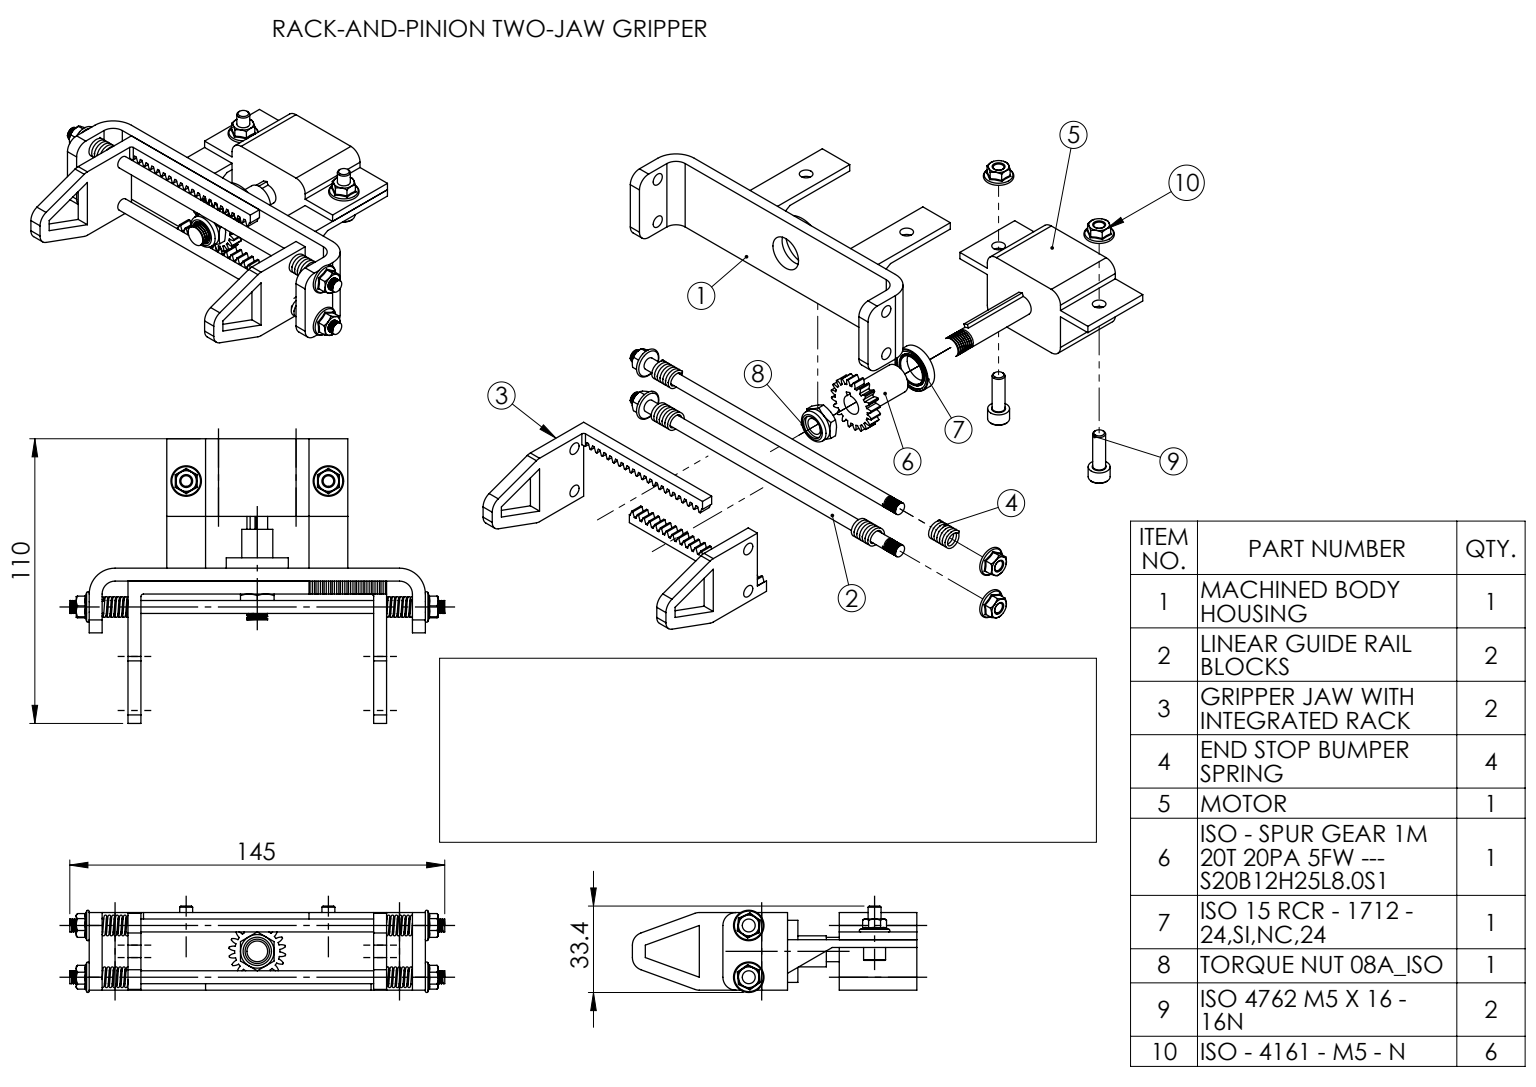
ISO-10303-21;
HEADER;
FILE_DESCRIPTION (('STEP AP214'),
    '1' );
FILE_NAME ('BR-005',
    '2026-10-08T13:46:47',
    ( '' ),
    ( '' ),
    'SwSTEP 2.0',
    'SolidWorks 2026',
    '' );
FILE_SCHEMA (( 'AUTOMOTIVE_DESIGN' ));
ENDSEC;

DATA;
#1 = CARTESIAN_POINT ( 'NONE',  ( -3.999999999999999112, 1.656854249492380804, 17.93750000000000711 ) ) ;
#2 = CARTESIAN_POINT ( 'NONE',  ( -4.000000000000000000, 0.9868501483902560878, -0.09357334158579519445 ) ) ;
#3 = VECTOR ( 'NONE', #11246, 1000.000000000000000 ) ;
#4 = CIRCLE ( 'NONE', #19877, 8.800000000000023803 ) ;
#5 = DIRECTION ( 'NONE',  ( -1.000000000000000000, 0.000000000000000000, -0.000000000000000000 ) ) ;
#6 = DIRECTION ( 'NONE',  ( -0.000000000000000000, -0.000000000000000000, 1.000000000000000000 ) ) ;
#7 = AXIS2_PLACEMENT_3D ( 'NONE', #19593, #12332, #12571 ) ;
#8 = CARTESIAN_POINT ( 'NONE',  ( -67.64999999999999147, 11.03553390593273598, 17.50000000000000355 ) ) ;
#9 = AXIS2_PLACEMENT_3D ( 'NONE', #7701, #5884, #15018 ) ;
#10 = DIRECTION ( 'NONE',  ( -0.000000000000000000, -0.000000000000000000, -1.000000000000000000 ) ) ;
#11 = CARTESIAN_POINT ( 'NONE',  ( 1.432654583217641164, 3.458734125000000326, 19.12500000136560629 ) ) ;
#12 = DIRECTION ( 'NONE',  ( 1.000000000000000000, 0.000000000000000000, 0.000000000000000000 ) ) ;
#13 = CARTESIAN_POINT ( 'NONE',  ( -1.656854249492380804, 4.000000000000000000, 6.112500000000002487 ) ) ;
#14 = ADVANCED_FACE ( 'NONE', ( #23177 ), #19348, .T. ) ;
#15 = DIRECTION ( 'NONE',  ( -1.000000000000000000, 0.000000000000000000, 0.000000000000000000 ) ) ;
#16 = CARTESIAN_POINT ( 'NONE',  ( 2.445694354108821855, -2.445694354108820079, 11.81250000136560629 ) ) ;
#17 = CARTESIAN_POINT ( 'NONE',  ( 65.80000000218494449, 9.999999999999998224, 12.49999999999999289 ) ) ;
#18 = ORIENTED_EDGE ( 'NONE', *, *, #6198, .T. ) ;
#19 = CARTESIAN_POINT ( 'NONE',  ( -69.15000000109247935, 8.538419263543524096, 13.53841926354352054 ) ) ;
#20 = ORIENTED_EDGE ( 'NONE', *, *, #20160, .F. ) ;
#21 = CARTESIAN_POINT ( 'NONE',  ( 57.71643183416158251, 13.97181229448536399, 16.72490539043799629 ) ) ;
#22 = CARTESIAN_POINT ( 'NONE',  ( -68.25000000109247367, 7.933012699999995476, 14.99999999999999645 ) ) ;
#23 = DIRECTION ( 'NONE',  ( 1.000000000000000000, 0.000000000000000000, 0.000000000000000000 ) ) ;
#24 = FACE_OUTER_BOUND ( 'NONE', #11980, .T. ) ;
#25 = VERTEX_POINT ( 'NONE', #5216 ) ;
#26 = VECTOR ( 'NONE', #20577, 1000.000000000000114 ) ;
#27 = EDGE_CURVE ( 'NONE', #6815, #4177, #10288, .T. ) ;
#28 =( GEOMETRIC_REPRESENTATION_CONTEXT ( 3 ) GLOBAL_UNCERTAINTY_ASSIGNED_CONTEXT ( ( #2821 ) ) GLOBAL_UNIT_ASSIGNED_CONTEXT ( ( #14742, #12246, #9459 ) ) REPRESENTATION_CONTEXT ( 'NONE', 'WORKASPACE' ) );
#29 = ORIENTED_EDGE ( 'NONE', *, *, #20734, .T. ) ;
#30 = CARTESIAN_POINT ( 'NONE',  ( -2.449293598294706907E-16, 4.000000000000000000, 7.613708498984758322 ) ) ;
#31 = CARTESIAN_POINT ( 'NONE',  ( 51.40856816583843880, 12.97181229448534978, 13.68930817193506755 ) ) ;
#32 = CARTESIAN_POINT ( 'NONE',  ( -70.40000000109250777, 10.85617417291294551, 17.06698729999999742 ) ) ;
#33 = CARTESIAN_POINT ( 'NONE',  ( -70.80000000109245661, 7.933012699999995476, 15.85617417291294196 ) ) ;
#34 = CARTESIAN_POINT ( 'NONE',  ( -1.432654583217639832, -3.458734125000000326, 12.87500000136560629 ) ) ;
#35 = DIRECTION ( 'NONE',  ( -1.000000000000000000, 0.000000000000000000, 0.000000000000000000 ) ) ;
#36 = CARTESIAN_POINT ( 'NONE',  ( 52.87500000000000711, 7.878679656440349177, 12.87867965644035984 ) ) ;
#37 = CIRCLE ( 'NONE', #17650, 6.543750000000021494 ) ;
#38 = DIRECTION ( 'NONE',  ( -0.000000000000000000, -0.000000000000000000, 1.000000000000000000 ) ) ;
#39 = CARTESIAN_POINT ( 'NONE',  ( 51.09375000000000000, 11.24264068711927322, 11.99999999999998934 ) ) ;
#40 = CARTESIAN_POINT ( 'NONE',  ( -3.999999999999999112, 0.000000000000000000, 16.12500000273119838 ) ) ;
#41 = CARTESIAN_POINT ( 'NONE',  ( -20.00000000000000711, 9.999999999999964473, -19.99999999999999645 ) ) ;
#42 = EDGE_LOOP ( 'NONE', ( #8288, #11668, #9814 ) ) ;
#43 = CARTESIAN_POINT ( 'NONE',  ( 70.34999999999999432, 7.499999999999996447, 13.96446609406725514 ) ) ;
#44 = CYLINDRICAL_SURFACE ( 'NONE', #19665, 4.000000000000000000 ) ;
#45 = ORIENTED_EDGE ( 'NONE', *, *, #7742, .T. ) ;
#46 = CARTESIAN_POINT ( 'NONE',  ( 51.56250000000000711, 6.999999999999997335, 15.00000000000000533 ) ) ;
#47 = CARTESIAN_POINT ( 'NONE',  ( -1.656854249492380804, 4.000000000000000000, -3.762499997268812013 ) ) ;
#48 = EDGE_CURVE ( 'NONE', #4600, #14452, #12227, .T. ) ;
#49 = DIRECTION ( 'NONE',  ( 1.000000000000000000, 0.000000000000000000, 0.000000000000000000 ) ) ;
#50 = ORIENTED_EDGE ( 'NONE', *, *, #19475, .F. ) ;
#51 = CARTESIAN_POINT ( 'NONE',  ( -3.999999999999999112, 1.656854249492380804, 17.93750000000000711 ) ) ;
#52 = CARTESIAN_POINT ( 'NONE',  ( 4.000000000000000000, 4.898587196589412829E-16, -2.199999999999998845 ) ) ;
#53 = CARTESIAN_POINT ( 'NONE',  ( 37.82128094071656932, -8.974600000000002353, 5.000000000000079936 ) ) ;
#54 = ORIENTED_EDGE ( 'NONE', *, *, #9397, .T. ) ;
#55 = LINE ( 'NONE', #5451, #11850 ) ;
#56 = LINE ( 'NONE', #21954, #15596 ) ;
#57 =( BOUNDED_CURVE ( )  B_SPLINE_CURVE ( 2, ( #2610, #2843, #8385, #9828, #929, #6582, #8267, #22849, #6463, #6101, #17122, #17483, #13433, #15701, #13784, #9954, #4303, #22975, #13896, #11639, #18906, #22618, #13542, #6222, #20810, #11753, #17248, #20493, #4334, #741, #505, #18828, #9508, #20729, #17161, #8185, #2415, #386, #851, #13111, #22409, #7826, #15148, #8076, #2169, #17043, #22169, #15387, #5783, #17285, #13469, #19061, #2652, #18588, #20845, #4223, #7945, #20371, #3977, #22286, #6018, #15031, #9746, #619, #18944, #15264, #9995, #7717, #11673, #4452, #2527, #5903, #11314, #13228, #4096, #9867, #13575, #16805, #11436, #18711, #22651, #22534, #2301, #9636, #6257, #16927, #11789, #11559, #13345, #20613, #6145, #10351, #23232, #4923, #21079, #10224, #15739, #2878, #3239, #19639, #8539, #1312, #13695, #13823, #19181, #20955, #6378, #23115, #17398, #12136, #14038, #23010, #4688, #12260, #8652, #1083, #8426, #10464, #2766, #17640, #1430, #6500, #17858, #21428, #22767, #13933, #19527, #15950, #1200 ),
 .UNSPECIFIED., .F., .F. ) 
 B_SPLINE_CURVE_WITH_KNOTS ( ( 3, 2, 2, 2, 2, 2, 2, 2, 2, 2, 2, 2, 2, 2, 2, 2, 2, 2, 2, 2, 2, 2, 2, 2, 2, 2, 2, 2, 2, 2, 2, 2, 2, 2, 2, 2, 2, 2, 2, 2, 2, 2, 2, 2, 2, 2, 2, 2, 2, 2, 2, 2, 2, 2, 2, 2, 2, 2, 2, 2, 2, 2, 2, 2, 3 ),
 ( 0.000000000000000000, 0.01562500000000000000, 0.03125000000000000000, 0.04687500000000000000, 0.06250000000000000000, 0.07812500000000000000, 0.09375000000000000000, 0.1093750000000000000, 0.1250000000000000000, 0.1406250000000000000, 0.1562500000000000000, 0.1718750000000000000, 0.1875000000000000000, 0.2031250000000000000, 0.2187500000000000000, 0.2343750000000000000, 0.2500000000000000000, 0.2656250000000000000, 0.2812500000000000000, 0.2968750000000000000, 0.3125000000000000000, 0.3281250000000000000, 0.3437500000000000000, 0.3593750000000000000, 0.3750000000000000000, 0.3906250000000000000, 0.4062500000000000000, 0.4218750000000000000, 0.4375000000000000000, 0.4531250000000000000, 0.4687500000000000000, 0.4843750000000000000, 0.5000000000000000000, 0.5156250000000000000, 0.5312500000000000000, 0.5468750000000000000, 0.5625000000000000000, 0.5781250000000000000, 0.5937500000000000000, 0.6093750000000000000, 0.6250000000000000000, 0.6406250000000000000, 0.6562500000000000000, 0.6718750000000000000, 0.6875000000000000000, 0.7031250000000000000, 0.7187500000000000000, 0.7343750000000000000, 0.7500000000000000000, 0.7656250000000000000, 0.7812500000000000000, 0.7968750000000000000, 0.8125000000000000000, 0.8281250000000000000, 0.8437500000000000000, 0.8593750000000000000, 0.8750000000000000000, 0.8906250000000000000, 0.9062500000000000000, 0.9218750000000000000, 0.9375000000000000000, 0.9531250000000000000, 0.9687500000000000000, 0.9843750000000000000, 1.000000000000000000 ),
 .UNSPECIFIED. ) 
 CURVE ( )  GEOMETRIC_REPRESENTATION_ITEM ( )  RATIONAL_B_SPLINE_CURVE ( ( 1.000000000000000000, 0.9238795325112867385, 1.000000000000000000, 0.9238795325112867385, 1.000000000000000000, 0.9238795325112867385, 1.000000000000000000, 0.9238795325112867385, 1.000000000000000000, 0.9238795325112867385, 1.000000000000000000, 0.9238795325112867385, 1.000000000000000000, 0.9238795325112867385, 1.000000000000000000, 0.9238795325112867385, 1.000000000000000000, 0.9238795325112867385, 1.000000000000000000, 0.9238795325112867385, 1.000000000000000000, 0.9238795325112867385, 1.000000000000000000, 0.9238795325112867385, 1.000000000000000000, 0.9238795325112867385, 1.000000000000000000, 0.9238795325112867385, 1.000000000000000000, 0.9238795325112867385, 1.000000000000000000, 0.9238795325112867385, 1.000000000000000000, 0.9238795325112867385, 1.000000000000000000, 0.9238795325112867385, 1.000000000000000000, 0.9238795325112867385, 1.000000000000000000, 0.9238795325112867385, 1.000000000000000000, 0.9238795325112867385, 1.000000000000000000, 0.9238795325112867385, 1.000000000000000000, 0.9238795325112867385, 1.000000000000000000, 0.9238795325112867385, 1.000000000000000000, 0.9238795325112867385, 1.000000000000000000, 0.9238795325112867385, 1.000000000000000000, 0.9238795325112867385, 1.000000000000000000, 0.9238795325112867385, 1.000000000000000000, 0.9238795325112867385, 1.000000000000000000, 0.9238795325112867385, 1.000000000000000000, 0.9238795325112867385, 1.000000000000000000, 0.9238795325112867385, 1.000000000000000000, 0.9238795325112867385, 1.000000000000000000, 0.9238795325112867385, 1.000000000000000000, 0.9238795325112867385, 1.000000000000000000, 0.9238795325112867385, 1.000000000000000000, 0.9238795325112867385, 1.000000000000000000, 0.9238795325112867385, 1.000000000000000000, 0.9238795325112867385, 1.000000000000000000, 0.9238795325112867385, 1.000000000000000000, 0.9238795325112867385, 1.000000000000000000, 0.9238795325112867385, 1.000000000000000000, 0.9238795325112867385, 1.000000000000000000, 0.9238795325112867385, 1.000000000000000000, 0.9238795325112867385, 1.000000000000000000, 0.9238795325112867385, 1.000000000000000000, 0.9238795325112867385, 1.000000000000000000, 0.9238795325112867385, 1.000000000000000000, 0.9238795325112867385, 1.000000000000000000, 0.9238795325112867385, 1.000000000000000000, 0.9238795325112867385, 1.000000000000000000, 0.9238795325112867385, 1.000000000000000000, 0.9238795325112867385, 1.000000000000000000, 0.9238795325112867385, 1.000000000000000000, 0.9238795325112867385, 1.000000000000000000, 0.9238795325112867385, 1.000000000000000000, 0.9238795325112867385, 1.000000000000000000, 0.9238795325112867385, 1.000000000000000000, 0.9238795325112867385, 1.000000000000000000, 0.9238795325112867385, 1.000000000000000000, 0.9238795325112867385, 1.000000000000000000, 0.9238795325112867385, 1.000000000000000000, 0.9238795325112867385, 1.000000000000000000, 0.9238795325112867385, 1.000000000000000000 ) ) 
 REPRESENTATION_ITEM ( '' )  );
#58 = CARTESIAN_POINT ( 'NONE',  ( 1.432654583217642053, -3.458734124999999882, 0.3000000013655960140 ) ) ;
#59 = CARTESIAN_POINT ( 'NONE',  ( 68.14999999999999147, 11.03553390593273598, 12.49999999999999289 ) ) ;
#60 = DIRECTION ( 'NONE',  ( -1.000000000000000000, -0.000000000000000000, 0.000000000000000000 ) ) ;
#61 = CARTESIAN_POINT ( 'NONE',  ( -4.000000000000000000, 4.898587196589412829E-16, 19.04999999999996874 ) ) ;
#62 = CARTESIAN_POINT ( 'NONE',  ( 52.25231816583844591, 7.219692298483957771, 17.87654654797633924 ) ) ;
#63 = CARTESIAN_POINT ( 'NONE',  ( 1.432654583217642275, -3.458734124999999437, -1.949999998634404319 ) ) ;
#64 = CARTESIAN_POINT ( 'NONE',  ( -2.445694354108819191, 2.445694354108820523, 10.31250000136560629 ) ) ;
#65 = DIRECTION ( 'NONE',  ( -1.000000000000000000, -0.000000000000000000, -0.000000000000000000 ) ) ;
#66 = CARTESIAN_POINT ( 'NONE',  ( 4.000000000000000000, 4.898587196589412829E-16, -0.1999999999999987899 ) ) ;
#67 = LINE ( 'NONE', #21968, #2877 ) ;
#68 = ORIENTED_EDGE ( 'NONE', *, *, #3329, .T. ) ;
#69 = PLANE ( 'NONE',  #9969 ) ;
#70 = CARTESIAN_POINT ( 'NONE',  ( -15.59503895323380362, -9.000000000000003553, 10.00000000000008882 ) ) ;
#71 = CARTESIAN_POINT ( 'NONE',  ( -72.37500000054622262, 9.999999999999998224, 17.28349365000000049 ) ) ;
#72 = ORIENTED_EDGE ( 'NONE', *, *, #3373, .F. ) ;
#73 = ORIENTED_EDGE ( 'NONE', *, *, #16986, .F. ) ;
#74 = DIRECTION ( 'NONE',  ( 0.000000000000000000, 0.000000000000000000, -1.000000000000000000 ) ) ;
#75 = CARTESIAN_POINT ( 'NONE',  ( 53.43750000000000711, 10.00000000000001776, 18.99999999999999645 ) ) ;
#76 = ORIENTED_EDGE ( 'NONE', *, *, #9529, .F. ) ;
#77 = LINE ( 'NONE', #11129, #17930 ) ;
#78 = ORIENTED_EDGE ( 'NONE', *, *, #18290, .F. ) ;
#79 = CARTESIAN_POINT ( 'NONE',  ( 56.84606816583843880, 8.411196891453267099, 19.02818770551464667 ) ) ;
#80 = AXIS2_PLACEMENT_3D ( 'NONE', #20688, #15213, #18897 ) ;
#81 = CARTESIAN_POINT ( 'NONE',  ( 66.15000000218495302, 11.03553390593273598, 17.50000000000000355 ) ) ;
#82 = ADVANCED_FACE ( 'NONE', ( #16139 ), #13987, .T. ) ;
#83 = DIRECTION ( 'NONE',  ( -1.000000000000000000, 0.000000000000000000, 0.000000000000000000 ) ) ;
#84 = CARTESIAN_POINT ( 'NONE',  ( -16.41397198033274307, -11.25000000000000355, 5.000000000000079936 ) ) ;
#85 = CARTESIAN_POINT ( 'NONE',  ( 2.828427124746190735, -2.828427124746189847, -0.3249999999999971800 ) ) ;
#86 = ORIENTED_EDGE ( 'NONE', *, *, #19557, .T. ) ;
#87 = CARTESIAN_POINT ( 'NONE',  ( -2.828427124746189403, 2.828427124746190291, 10.87500000000001066 ) ) ;
#88 = DIRECTION ( 'NONE',  ( 0.3420201433256622181, 0.9396926207859107594, -6.162975822039141593E-32 ) ) ;
#89 = CARTESIAN_POINT ( 'NONE',  ( 52.27893183416158251, 8.411196891453236901, 10.97181229448535511 ) ) ;
#90 = PLANE ( 'NONE',  #415 ) ;
#91 = EDGE_CURVE ( 'NONE', #13267, #15347, #17804, .T. ) ;
#92 = DIRECTION ( 'NONE',  ( 0.000000000000000000, 0.000000000000000000, -1.000000000000000000 ) ) ;
#93 = CARTESIAN_POINT ( 'NONE',  ( 72.25000000000000000, 12.50000000000000000, 13.96446609406725692 ) ) ;
#94 = LINE ( 'NONE', #22476, #8071 ) ;
#95 = ORIENTED_EDGE ( 'NONE', *, *, #9004, .T. ) ;
#96 = DIRECTION ( 'NONE',  ( -1.000000000000000000, -0.000000000000000000, -0.000000000000000000 ) ) ;
#97 = CARTESIAN_POINT ( 'NONE',  ( 53.25000000000000711, 7.878679656440361612, 17.12132034355964549 ) ) ;
#98 = LINE ( 'NONE', #14992, #12792 ) ;
#99 =( NAMED_UNIT ( * ) PLANE_ANGLE_UNIT ( ) SI_UNIT ( $, .RADIAN. ) );
#100 = ORIENTED_EDGE ( 'NONE', *, *, #5298, .F. ) ;
#101 = DIRECTION ( 'NONE',  ( -0.9396926207859107594, -0.3420201433256623291, 1.540743955509804830E-32 ) ) ;
#102 = LINE ( 'NONE', #22483, #7227 ) ;
#103 = DIRECTION ( 'NONE',  ( 1.224646799147353207E-16, -0.000000000000000000, 1.000000000000000000 ) ) ;
#104 = ORIENTED_EDGE ( 'NONE', *, *, #7323, .T. ) ;
#105 = CARTESIAN_POINT ( 'NONE',  ( 69.74999999999998579, 11.03553390593276262, 12.50000000000001776 ) ) ;
#106 = EDGE_LOOP ( 'NONE', ( #16635, #20382, #2451, #21476 ) ) ;
#107 = CARTESIAN_POINT ( 'NONE',  ( -65.40000000218495302, 9.999999999999998224, 17.49999999999999645 ) ) ;
#108 = CARTESIAN_POINT ( 'NONE',  ( 4.000000000000000888, 4.898587196589412829E-16, 18.50000000000001066 ) ) ;
#109 = CARTESIAN_POINT ( 'NONE',  ( -1.594879469667249916, -11.25000000000000355, 5.000000000000079936 ) ) ;
#110 = EDGE_CURVE ( 'NONE', #1631, #9768, #19532, .T. ) ;
#111 = DIRECTION ( 'NONE',  ( 0.5000000000000006661, 0.8660254037844382635, -0.000000000000000000 ) ) ;
#112 = EDGE_CURVE ( 'NONE', #23518, #15611, #3206, .T. ) ;
#113 = CARTESIAN_POINT ( 'NONE',  ( -3.462118672051860191, 1.261024841198670421, -3.429387741257551081 ) ) ;
#114 =( NAMED_UNIT ( * ) PLANE_ANGLE_UNIT ( ) SI_UNIT ( $, .RADIAN. ) );
#115 = ORIENTED_EDGE ( 'NONE', *, *, #19552, .T. ) ;
#116 = CARTESIAN_POINT ( 'NONE',  ( -66.74999999999998579, 12.50000000000000000, 16.03553390593273420 ) ) ;
#117 = AXIS2_PLACEMENT_3D ( 'NONE', #18833, #4695, #4456 ) ;
#118 = CARTESIAN_POINT ( 'NONE',  ( 66.45000000218495018, 7.499999999999996447, 13.96446609406725514 ) ) ;
#119 = EDGE_CURVE ( 'NONE', #21784, #14801, #1618, .T. ) ;
#120 = CARTESIAN_POINT ( 'NONE',  ( 65.80000000109247082, 7.933012699999995476, 15.85617417291294196 ) ) ;
#121 = CARTESIAN_POINT ( 'NONE',  ( 1.025207404391860050E-15, 3.458734125000000326, 19.18750000136560629 ) ) ;
#122 = DIRECTION ( 'NONE',  ( -1.000000000000000000, -0.000000000000000000, 0.000000000000000000 ) ) ;
#123 = CARTESIAN_POINT ( 'NONE',  ( -4.000000000000000000, 0.000000000000000000, 5.300000000000000711 ) ) ;
#124 = CARTESIAN_POINT ( 'NONE',  ( -3.999999999999999112, 0.000000000000000000, 13.00000000000001066 ) ) ;
#125 = CARTESIAN_POINT ( 'NONE',  ( 1.432654583217641164, 3.458734125000000326, 12.12500000136560629 ) ) ;
#126 = DIRECTION ( 'NONE',  ( 0.000000000000000000, 0.5877852522924743583, -0.8090169943749467851 ) ) ;
#127 = PRODUCT ( 'Linear Guide Rail Blocks', 'Linear Guide Rail Blocks', '', ( #7707 ) ) ;
#128 =( REPRESENTATION_RELATIONSHIP ('NONE','NONE', #8403, #16640 ) REPRESENTATION_RELATIONSHIP_WITH_TRANSFORMATION ( #23106 )SHAPE_REPRESENTATION_RELATIONSHIP( ) );
#129 = VERTEX_POINT ( 'NONE', #3181 ) ;
#130 = CARTESIAN_POINT ( 'NONE',  ( -70.65000000109247935, 7.933012699999995476, 14.99999999999999645 ) ) ;
#131 = ORIENTED_EDGE ( 'NONE', *, *, #16683, .F. ) ;
#132 = CARTESIAN_POINT ( 'NONE',  ( 56.49768183416158962, 12.87654654797631792, 12.21969229848393113 ) ) ;
#133 = CARTESIAN_POINT ( 'NONE',  ( -69.95000000109247651, 8.538419263543522320, 16.46158073645647235 ) ) ;
#134 = DIRECTION ( 'NONE',  ( 0.3420201433256622736, -0.9396926207859106484, -1.232595164407828100E-31 ) ) ;
#135 = ORIENTED_EDGE ( 'NONE', *, *, #23501, .F. ) ;
#136 = CIRCLE ( 'NONE', #7427, 8.749000000000002331 ) ;
#137 = EDGE_CURVE ( 'NONE', #15758, #669, #1279, .T. ) ;
#138 = ORIENTED_EDGE ( 'NONE', *, *, #22563, .F. ) ;
#139 = CARTESIAN_POINT ( 'NONE',  ( 1.025207404391860050E-15, 3.458734125000000770, 19.43750000136560629 ) ) ;
#140 = CARTESIAN_POINT ( 'NONE',  ( 50.84606816583843880, 8.825410453826357582, 18.02818770551464667 ) ) ;
#141 = CARTESIAN_POINT ( 'NONE',  ( -70.30000000109248504, 12.06698730000000275, 15.85617417291294196 ) ) ;
#142 = ADVANCED_FACE ( 'NONE', ( #17693 ), #8211, .T. ) ;
#143 = AXIS2_PLACEMENT_3D ( 'NONE', #14347, #4748, #19821 ) ;
#144 = CARTESIAN_POINT ( 'NONE',  ( -68.90000000109246514, 12.06698730000000275, 15.85617417291294196 ) ) ;
#145 = DIRECTION ( 'NONE',  ( 1.000000000000000000, 0.000000000000000000, 0.000000000000000000 ) ) ;
#146 = CARTESIAN_POINT ( 'NONE',  ( -4.197393957002303999, -0.8151795401431414234, -3.503767560748935139 ) ) ;
#147 = EDGE_CURVE ( 'NONE', #12600, #6989, #10767, .T. ) ;
#148 = CARTESIAN_POINT ( 'NONE',  ( 52.59375000000000711, 11.24264068711927322, 11.99999999999998934 ) ) ;
#149 = DIRECTION ( 'NONE',  ( -0.000000000000000000, 1.000000000000000000, -0.000000000000000000 ) ) ;
#150 = ADVANCED_FACE ( 'NONE', ( #6674 ), #1255, .T. ) ;
#151 = CARTESIAN_POINT ( 'NONE',  ( 53.53125000000000000, 11.24264068711929276, 18.00000000000000355 ) ) ;
#152 = CARTESIAN_POINT ( 'NONE',  ( 2.828427124746191179, 2.828427124746190291, 16.75000000273119838 ) ) ;
#153 = CIRCLE ( 'NONE', #6290, 4.000000000000001776 ) ;
#154 = CARTESIAN_POINT ( 'NONE',  ( 0.000000000000000000, -6.807171995660630692, 6.478011392632865295 ) ) ;
#155 = ORIENTED_EDGE ( 'NONE', *, *, #6433, .T. ) ;
#156 = PLANE ( 'NONE',  #640 ) ;
#157 = DIRECTION ( 'NONE',  ( 0.000000000000000000, -0.5000000000000013323, -0.8660254037844380415 ) ) ;
#158 = VERTEX_POINT ( 'NONE', #14232 ) ;
#159 = CARTESIAN_POINT ( 'NONE',  ( 56.53125000000000711, 11.24264068711929276, 18.00000000000000355 ) ) ;
#160 = SHAPE_REPRESENTATION_RELATIONSHIP ( 'NONE' , 'NONE' ,  #21657, #23316 ) ;
#161 = CARTESIAN_POINT ( 'NONE',  ( -4.000000000000000000, 0.000000000000000000, -3.574999997268813345 ) ) ;
#162 = CARTESIAN_POINT ( 'NONE',  ( 0.000000000000000000, 8.734705317681626724, 0.4999240074894746311 ) ) ;
#163 = EDGE_LOOP ( 'NONE', ( #11926, #9708, #6526, #4328 ) ) ;
#164 = CARTESIAN_POINT ( 'NONE',  ( 1.971781867644420635E-15, -4.000000000000000000, 16.25000000000001066 ) ) ;
#165 = CARTESIAN_POINT ( 'NONE',  ( 0.000000000000000000, 0.4999240074895661690, -8.734705317681621395 ) ) ;
#166 = CARTESIAN_POINT ( 'NONE',  ( 4.999999999999999112, 8.734705317681626724, -0.4999240074894757413 ) ) ;
#167 = ORIENTED_EDGE ( 'NONE', *, *, #18888, .T. ) ;
#168 = DIRECTION ( 'NONE',  ( 0.3420201433256622181, 0.9396926207859107594, -6.162975822039141593E-32 ) ) ;
#169 = DIRECTION ( 'NONE',  ( -1.000000000000000000, 0.000000000000000000, 0.000000000000000000 ) ) ;
#170 = CARTESIAN_POINT ( 'NONE',  ( 67.99999999999998579, 8.232233047033629347, 13.23223304703362402 ) ) ;
#171 = ADVANCED_FACE ( 'NONE', ( #19699 ), #12685, .T. ) ;
#172 = DIRECTION ( 'NONE',  ( 0.000000000000000000, 0.000000000000000000, 1.000000000000000000 ) ) ;
#173 = AXIS2_PLACEMENT_3D ( 'NONE', #18053, #16495, #3661 ) ;
#174 = EDGE_CURVE ( 'NONE', #22879, #11902, #20401, .T. ) ;
#176 = CARTESIAN_POINT ( 'NONE',  ( -1.317756351988340180, 3.857995168970202116, -0.04852650426601388955 ) ) ;
#175 = AXIS2_PLACEMENT_3D ( 'NONE', #8755, #4676, #12125 ) ;
#177 = CARTESIAN_POINT ( 'NONE',  ( 52.43981816583844591, 10.06805114094564857, 19.00000000000000000 ) ) ;
#178 = AXIS2_PLACEMENT_3D ( 'NONE', #2507, #15364, #6234 ) ;
#179 = CARTESIAN_POINT ( 'NONE',  ( -2.445694354108819635, -2.445694354108820523, -1.137499998634402765 ) ) ;
#180 = CARTESIAN_POINT ( 'NONE',  ( 3.458734125000002546, -1.432654583217639610, 15.12500000136560807 ) ) ;
#181 = CARTESIAN_POINT ( 'NONE',  ( 68.60000000218495586, 9.999999999999998224, 17.49999999999999645 ) ) ;
#182 = CARTESIAN_POINT ( 'NONE',  ( 2.500000000000000000, -1.178949249685214307, 2.042000000000001592 ) ) ;
#183 = CARTESIAN_POINT ( 'NONE',  ( 9.920644283265380691E-16, 4.000000000000000000, 16.75000000000001066 ) ) ;
#184 = ORIENTED_EDGE ( 'NONE', *, *, #1140, .T. ) ;
#185 = CARTESIAN_POINT ( 'NONE',  ( 1.656854249492381470, 4.000000000000000000, 11.81250000273119660 ) ) ;
#186 = DIRECTION ( 'NONE',  ( 1.000000000000000000, 7.703719777548943412E-32, 0.000000000000000000 ) ) ;
#187 = DIRECTION ( 'NONE',  ( 0.9396926207859107594, -0.3420201433256623291, 3.697785493223492838E-32 ) ) ;
#188 = EDGE_LOOP ( 'NONE', ( #20058, #4346, #18980, #11606 ) ) ;
#189 = ORIENTED_EDGE ( 'NONE', *, *, #1029, .F. ) ;
#190 = LINE ( 'NONE', #7521, #665 ) ;
#191 =( BOUNDED_CURVE ( )  B_SPLINE_CURVE ( 2, ( #20921, #4538, #19693, #10520, #10408, #17688, #1250, #8589, #23173 ),
 .UNSPECIFIED., .F., .F. ) 
 B_SPLINE_CURVE_WITH_KNOTS ( ( 3, 2, 2, 2, 3 ),
 ( 0.3125000000000002776, 0.3281250000000001665, 0.3437500000000001110, 0.3593750000000000000, 0.3749999999999998890 ),
 .UNSPECIFIED. ) 
 CURVE ( )  GEOMETRIC_REPRESENTATION_ITEM ( )  RATIONAL_B_SPLINE_CURVE ( ( 0.9999999999999986677, 0.9238795325112880708, 1.000000000000000000, 0.9238795325112867385, 1.000000000000000000, 0.9238795325112867385, 1.000000000000000000, 0.9238795325112872936, 0.9999999999999994449 ) ) 
 REPRESENTATION_ITEM ( '' )  );
#192 = CARTESIAN_POINT ( 'NONE',  ( 58.59375000000000711, 11.65685424949236015, 10.99999999999998579 ) ) ;
#193 = ORIENTED_EDGE ( 'NONE', *, *, #20761, .T. ) ;
#194 = CARTESIAN_POINT ( 'NONE',  ( -2.828427124746188515, -2.828427124746190735, 18.12500000000001066 ) ) ;
#195 = ORIENTED_EDGE ( 'NONE', *, *, #4034, .T. ) ;
#196 = CARTESIAN_POINT ( 'NONE',  ( 54.97106816583843880, 5.971812294485345340, 13.41119689145326710 ) ) ;
#197 = AXIS2_PLACEMENT_3D ( 'NONE', #16444, #18702, #9272 ) ;
#198 = CARTESIAN_POINT ( 'NONE',  ( 70.50000000109247367, 9.143825827087049163, 17.06698729999999742 ) ) ;
#199 = CARTESIAN_POINT ( 'NONE',  ( -2.000000000000001776, 8.130889342088984924E-16, 6.543750000000021494 ) ) ;
#200 = CARTESIAN_POINT ( 'NONE',  ( 70.75000000109247367, 8.538419263543522320, 16.46158073645647235 ) ) ;
#201 = ORIENTED_EDGE ( 'NONE', *, *, #13509, .T. ) ;
#202 = CARTESIAN_POINT ( 'NONE',  ( 9.920644283265380691E-16, 4.000000000000000000, 15.87500000273119660 ) ) ;
#203 = CARTESIAN_POINT ( 'NONE',  ( -2.449293598294706907E-16, 4.000000000000000000, 0.1750000027311865991 ) ) ;
#204 = CARTESIAN_POINT ( 'NONE',  ( 56.49768183416158962, 12.87654654797631792, 12.21969229848393113 ) ) ;
#205 = CARTESIAN_POINT ( 'NONE',  ( 33.85151041966726382, -11.25000000000000355, 5.000000000000079936 ) ) ;
#206 = DIRECTION ( 'NONE',  ( -1.000000000000000000, -0.000000000000000000, -0.000000000000000000 ) ) ;
#207 = CARTESIAN_POINT ( 'NONE',  ( -2.762848947613220307, 4.746226468750993632, -19.99999999999999645 ) ) ;
#208 = CARTESIAN_POINT ( 'NONE',  ( 4.000000000000000000, -2.471525695159793035, -3.686886880705770864 ) ) ;
#209 = ORIENTED_EDGE ( 'NONE', *, *, #10563, .F. ) ;
#210 = LINE ( 'NONE', #7541, #1252 ) ;
#211 = CARTESIAN_POINT ( 'NONE',  ( -4.000000000000000000, -0.8232339106130515116, -3.430630286862743183 ) ) ;
#212 = AXIS2_PLACEMENT_3D ( 'NONE', #2091, #18271, #1855 ) ;
#213 = DIRECTION ( 'NONE',  ( -1.000000000000000000, -0.000000000000000000, 0.000000000000000000 ) ) ;
#214 = PRESENTATION_STYLE_ASSIGNMENT (( #11263 ) ) ;
#215 = ORIENTED_EDGE ( 'NONE', *, *, #13747, .F. ) ;
#216 = EDGE_CURVE ( 'NONE', #1719, #20740, #5490, .T. ) ;
#217 = DIRECTION ( 'NONE',  ( 1.000000000000000000, 0.000000000000000000, 0.000000000000000000 ) ) ;
#218 = CARTESIAN_POINT ( 'NONE',  ( 70.54999999999999716, 11.03553390593272177, 12.49999999999998046 ) ) ;
#219 = CARTESIAN_POINT ( 'NONE',  ( 5.000000000000002665, 3.306546357697854226E-16, 2.700000000000000622 ) ) ;
#220 = DIRECTION ( 'NONE',  ( 1.000000000000000000, -0.000000000000000000, -0.000000000000000000 ) ) ;
#221 = ORIENTED_EDGE ( 'NONE', *, *, #20920, .F. ) ;
#222 = CARTESIAN_POINT ( 'NONE',  ( 4.000000000000000000, 2.309401076758497151, -3.433295621305379353 ) ) ;
#223 = ORIENTED_EDGE ( 'NONE', *, *, #14244, .T. ) ;
#224 = CARTESIAN_POINT ( 'NONE',  ( -19.99999999999999645, -9.000000000000003553, 5.000000000000079936 ) ) ;
#225 = CARTESIAN_POINT ( 'NONE',  ( 4.000000000000000888, 4.898587196589412829E-16, 15.50000000000001066 ) ) ;
#226 = DIRECTION ( 'NONE',  ( -1.000000000000000000, -0.000000000000000000, 0.000000000000000000 ) ) ;
#227 = FACE_OUTER_BOUND ( 'NONE', #6243, .T. ) ;
#228 = DIRECTION ( 'NONE',  ( 0.000000000000000000, 0.000000000000000000, -1.000000000000000000 ) ) ;
#229 = CARTESIAN_POINT ( 'NONE',  ( 71.25000000109247367, 12.06698730000000097, 14.99999999999999645 ) ) ;
#230 = ORIENTED_EDGE ( 'NONE', *, *, #2307, .F. ) ;
#231 = CARTESIAN_POINT ( 'NONE',  ( -68.54999999999999716, 8.964466094067258695, 17.50000000000000355 ) ) ;
#232 = DIRECTION ( 'NONE',  ( -0.000000000000000000, -0.000000000000000000, 1.000000000000000000 ) ) ;
#233 = CARTESIAN_POINT ( 'NONE',  ( 66.95000000109246230, 11.46158073645647235, 13.53841926354352232 ) ) ;
#234 = CARTESIAN_POINT ( 'NONE',  ( 1.432654583217643163, -3.458734124999999437, 15.75000000136560629 ) ) ;
#235 = CARTESIAN_POINT ( 'NONE',  ( -4.898587196589412829E-16, 0.000000000000000000, -4.000000000000000000 ) ) ;
#236 = CARTESIAN_POINT ( 'NONE',  ( 1.432654583217642275, -3.458734124999999882, -2.699999998634404541 ) ) ;
#237 = CARTESIAN_POINT ( 'NONE',  ( -2.828427124746190291, 2.828427124746190291, 6.175000000000001599 ) ) ;
#238 = CARTESIAN_POINT ( 'NONE',  ( -3.458734124999998993, 1.432654583217640276, 12.37500000136560629 ) ) ;
#239 = DIRECTION ( 'NONE',  ( -1.000000000000000000, 0.000000000000000000, 0.000000000000000000 ) ) ;
#240 = ORIENTED_EDGE ( 'NONE', *, *, #11094, .F. ) ;
#241 = EDGE_CURVE ( 'NONE', #1931, #14063, #136, .T. ) ;
#242 = CARTESIAN_POINT ( 'NONE',  ( -69.65000000109247935, 9.999999999999998224, 17.06698730000000097 ) ) ;
#243 = ORIENTED_EDGE ( 'NONE', *, *, #7766, .T. ) ;
#244 = CARTESIAN_POINT ( 'NONE',  ( 55.93518183416157541, 9.931948859054379852, 18.99999999999999289 ) ) ;
#245 = CARTESIAN_POINT ( 'NONE',  ( -71.80000000109245661, 9.143825827087050939, 12.93301269999999370 ) ) ;
#246 = APPLICATION_PROTOCOL_DEFINITION ( 'draft international standard', 'automotive_design', 1998, #4859 ) ;
#247 = EDGE_CURVE ( 'NONE', #438, #3610, #9877, .T. ) ;
#248 = LINE ( 'NONE', #7582, #20083 ) ;
#249 = ORIENTED_EDGE ( 'NONE', *, *, #5499, .T. ) ;
#250 = ORIENTED_EDGE ( 'NONE', *, *, #1042, .T. ) ;
#251 = CARTESIAN_POINT ( 'NONE',  ( 3.458734125000001658, 1.432654583217640498, 17.25000000136560629 ) ) ;
#252 = EDGE_CURVE ( 'NONE', #16322, #3084, #16594, .T. ) ;
#253 = CARTESIAN_POINT ( 'NONE',  ( 54.56250000000000711, 6.999999999999997335, 15.00000000000000533 ) ) ;
#254 = CARTESIAN_POINT ( 'NONE',  ( -70.50000000109247367, 9.143825827087049163, 17.06698729999999742 ) ) ;
#255 = CIRCLE ( 'NONE', #4097, 8.749000000000002331 ) ;
#256 = CARTESIAN_POINT ( 'NONE',  ( -69.15000000109246514, 8.538419263543522320, 16.46158073645647235 ) ) ;
#257 = CARTESIAN_POINT ( 'NONE',  ( 3.458734125000001658, 1.432654583217640498, 13.25000000136560274 ) ) ;
#258 = PLANE ( 'NONE',  #11121 ) ;
#259 = CARTESIAN_POINT ( 'NONE',  ( 59.96643183416158251, 7.028187705514638672, 13.68930817193508531 ) ) ;
#260 = CARTESIAN_POINT ( 'NONE',  ( -71.70000000000000284, 9.999999999999998224, 17.49999999999999645 ) ) ;
#261 =( REPRESENTATION_RELATIONSHIP ('NONE','NONE', #8403, #20612 ) REPRESENTATION_RELATIONSHIP_WITH_TRANSFORMATION ( #13103 )SHAPE_REPRESENTATION_RELATIONSHIP( ) );
#262 = CARTESIAN_POINT ( 'NONE',  ( 54.28125000000000000, 8.757359312880703683, 11.99999999999999822 ) ) ;
#263 = CARTESIAN_POINT ( 'NONE',  ( -1.432654583217638944, 3.458734125000000326, 12.25000000136560629 ) ) ;
#264 = CARTESIAN_POINT ( 'NONE',  ( 4.000000000000001776, -1.656854249492379694, 16.56250000273119838 ) ) ;
#265 = DIRECTION ( 'NONE',  ( -1.000000000000000000, 0.000000000000000000, 0.000000000000000000 ) ) ;
#266 = AXIS2_PLACEMENT_3D ( 'NONE', #5948, #13273, #13627 ) ;
#267 = AXIS2_PLACEMENT_3D ( 'NONE', #23534, #5337, #9303 ) ;
#268 = EDGE_LOOP ( 'NONE', ( #17451, #14337, #19038, #18297, #4703 ) ) ;
#269 = CARTESIAN_POINT ( 'NONE',  ( 5.200000000000002842, 0.000000000000000000, 0.000000000000000000 ) ) ;
#270 = EDGE_CURVE ( 'NONE', #13563, #6956, #18497, .T. ) ;
#271 = CYLINDRICAL_SURFACE ( 'NONE', #5922, 4.714285714285714413 ) ;
#272 = ORIENTED_EDGE ( 'NONE', *, *, #1937, .F. ) ;
#273 = CARTESIAN_POINT ( 'NONE',  ( 56.15625000000002132, 7.000000000000003553, 16.24264068711929099 ) ) ;
#274 = CARTESIAN_POINT ( 'NONE',  ( 3.458734125000000770, -1.432654583217639610, 4.175000001365593683 ) ) ;
#275 = ADVANCED_FACE ( 'NONE', ( #14703 ), #22200, .F. ) ;
#276 = FACE_OUTER_BOUND ( 'NONE', #8026, .T. ) ;
#277 = EDGE_LOOP ( 'NONE', ( #17839, #20951 ) ) ;
#278 = CARTESIAN_POINT ( 'NONE',  ( 4.000000000000001776, -1.656854249492379694, 13.43750000000001243 ) ) ;
#279 = LINE ( 'NONE', #14812, #13339 ) ;
#280 = LINE ( 'NONE', #14938, #18655 ) ;
#281 = ORIENTED_EDGE ( 'NONE', *, *, #12290, .F. ) ;
#282 = ADVANCED_FACE ( 'NONE', ( #9074 ), #16365, .T. ) ;
#283 = ADVANCED_FACE ( 'NONE', ( #1848 ), #11347, .T. ) ;
#284 = VECTOR ( 'NONE', #13283, 1000.000000000000000 ) ;
#285 = DIRECTION ( 'NONE',  ( -0.000000000000000000, -0.000000000000000000, -1.000000000000000000 ) ) ;
#286 = DIRECTION ( 'NONE',  ( 0.000000000000000000, 0.000000000000000000, -1.000000000000000000 ) ) ;
#287 = AXIS2_PLACEMENT_3D ( 'NONE', #3170, #5332, #9063 ) ;
#288 = AXIS2_PLACEMENT_3D ( 'NONE', #14869, #22247, #466 ) ;
#289 = CARTESIAN_POINT ( 'NONE',  ( 69.14999999999999147, 12.50000000000000000, 16.03553390593273420 ) ) ;
#290 = FACE_OUTER_BOUND ( 'NONE', #18662, .T. ) ;
#291 = DIRECTION ( 'NONE',  ( -1.000000000000000000, 0.000000000000000000, 0.000000000000000000 ) ) ;
#292 = CARTESIAN_POINT ( 'NONE',  ( 59.00231816583843170, 12.07320092032949610, 12.83056023321021044 ) ) ;
#293 = CARTESIAN_POINT ( 'NONE',  ( 3.458734125000000326, 1.432654583217640498, 0.3000000013655960696 ) ) ;
#294 = CARTESIAN_POINT ( 'NONE',  ( 1.432654583217641386, 3.458734125000000770, 13.37500000136560452 ) ) ;
#295 = CARTESIAN_POINT ( 'NONE',  ( 0.000000000000000000, -10.82112760146737962, 1.975651141462196225 ) ) ;
#296 = DIRECTION ( 'NONE',  ( -0.000000000000000000, -1.000000000000000000, -0.000000000000000000 ) ) ;
#297 = VECTOR ( 'NONE', #11394, 1000.000000000000000 ) ;
#298 = CARTESIAN_POINT ( 'NONE',  ( -2.500000000000000444, 3.061616997868383634E-16, -5.000000000000000888 ) ) ;
#299 = VERTEX_POINT ( 'NONE', #11106 ) ;
#300 = DIRECTION ( 'NONE',  ( 0.000000000000000000, 0.000000000000000000, -1.000000000000000000 ) ) ;
#301 = DIRECTION ( 'NONE',  ( -1.000000000000000000, -0.000000000000000000, -0.000000000000000000 ) ) ;
#302 = EDGE_CURVE ( 'NONE', #23443, #22486, #15470, .T. ) ;
#303 = CARTESIAN_POINT ( 'NONE',  ( -2.247776618166699603, 3.308700692843501656, 21.31370849898476649 ) ) ;
#304 = ORIENTED_EDGE ( 'NONE', *, *, #3176, .T. ) ;
#305 = B_SPLINE_CURVE_WITH_KNOTS ( 'NONE', 3,
 ( #22141, #7915, #17258, #22261, #2503 ),
 .UNSPECIFIED., .F., .F.,
 ( 4, 1, 4 ),
 ( 0.000000000000000000, 0.002309401076758506657, 0.004618802153517013315 ),
 .UNSPECIFIED. ) ;
#306 = AXIS2_PLACEMENT_3D ( 'NONE', #17570, #1367, #5089 ) ;
#307 = ORIENTED_EDGE ( 'NONE', *, *, #9563, .T. ) ;
#308 = AXIS2_PLACEMENT_3D ( 'NONE', #22558, #8314, #14060 ) ;
#309 = FILL_AREA_STYLE ('',( #2348 ) ) ;
#310 = EDGE_CURVE ( 'NONE', #17992, #7710, #5573, .T. ) ;
#311 = PRESENTATION_LAYER_ASSIGNMENT (  '', '', ( #14103 ) ) ;
#312 = CARTESIAN_POINT ( 'NONE',  ( 54.37500000000000711, 7.171572875253794166, 12.17157287525381726 ) ) ;
#313 = VERTEX_POINT ( 'NONE', #3887 ) ;
#314 = CARTESIAN_POINT ( 'NONE',  ( -6.500000000000000000, -3.752776749732573247, -0.5805565836007695601 ) ) ;
#315 = VERTEX_POINT ( 'NONE', #10985 ) ;
#316 = EDGE_CURVE ( 'NONE', #22906, #15640, #20161, .T. ) ;
#317 = CARTESIAN_POINT ( 'NONE',  ( 51.78356816583844591, 8.275094609561968184, 11.02818770551464667 ) ) ;
#318 = CARTESIAN_POINT ( 'NONE',  ( 70.70000000109247651, 7.933012699999995476, 14.14382582708705094 ) ) ;
#319 = CARTESIAN_POINT ( 'NONE',  ( 66.49999999999998579, 9.999999999999998224, 12.49999999999999289 ) ) ;
#320 = CARTESIAN_POINT ( 'NONE',  ( 71.55000000109245661, 8.538419263543522320, 16.46158073645647235 ) ) ;
#321 = PRODUCT_DEFINITION_SHAPE ( 'NONE', 'NONE',  #23701 ) ;
#322 = ORIENTED_EDGE ( 'NONE', *, *, #7035, .T. ) ;
#323 = CARTESIAN_POINT ( 'NONE',  ( 1.656854249492384135, -3.999999999999999112, 17.43750000273119483 ) ) ;
#324 = CARTESIAN_POINT ( 'NONE',  ( -2.828427124746190291, 2.828427124746190291, 0.3000000027311867101 ) ) ;
#325 = VECTOR ( 'NONE', #2577, 1000.000000000000000 ) ;
#326 = CARTESIAN_POINT ( 'NONE',  ( 53.21643183416158251, 13.97181229448536399, 16.72490539043799629 ) ) ;
#327 = CARTESIAN_POINT ( 'NONE',  ( 40.13469571966727045, -11.25000000000000355, 10.00000000000008882 ) ) ;
#328 = CARTESIAN_POINT ( 'NONE',  ( 2.499999999999999556, 1.464956435139542323, 10.90201369670499076 ) ) ;
#329 = CARTESIAN_POINT ( 'NONE',  ( 27.50000000000000000, 1.500000000000003109, -33.66025403784446723 ) ) ;
#330 = CARTESIAN_POINT ( 'NONE',  ( 1.656854249492383024, -3.999999999999999112, 0.6125000000000022649 ) ) ;
#331 = CARTESIAN_POINT ( 'NONE',  ( -1.301042606982605321E-15, 7.505553499465137612, -0.5805565836007695601 ) ) ;
#332 = ORIENTED_EDGE ( 'NONE', *, *, #12450, .T. ) ;
#333 = CARTESIAN_POINT ( 'NONE',  ( -70.20000000218495018, 9.999999999999998224, 17.49999999999999645 ) ) ;
#334 = CARTESIAN_POINT ( 'NONE',  ( -4.211399284164270895, 2.459729995988205964, -3.751162237960538715 ) ) ;
#335 = FACE_OUTER_BOUND ( 'NONE', #5328, .T. ) ;
#336 = AXIS2_PLACEMENT_3D ( 'NONE', #17862, #16313, #17643 ) ;
#337 = ORIENTED_EDGE ( 'NONE', *, *, #22086, .T. ) ;
#338 = VECTOR ( 'NONE', #6203, 1000.000000000000000 ) ;
#339 = CARTESIAN_POINT ( 'NONE',  ( 4.999999999999999112, 0.000000000000000000, 0.000000000000000000 ) ) ;
#340 = CARTESIAN_POINT ( 'NONE',  ( -19.99999999999999645, -9.000000000000003553, 5.000000000000079936 ) ) ;
#341 = DIRECTION ( 'NONE',  ( 1.000000000000000000, 0.000000000000000000, 0.000000000000000000 ) ) ;
#342 = EDGE_CURVE ( 'NONE', #20113, #6042, #11222, .T. ) ;
#343 = CARTESIAN_POINT ( 'NONE',  ( 1.656854249492384135, -3.999999999999999112, 16.43750000273119838 ) ) ;
#344 = ORIENTED_EDGE ( 'NONE', *, *, #2171, .T. ) ;
#345 = CARTESIAN_POINT ( 'NONE',  ( -4.471005642132689140, -3.347908285648603766, 10.00000000000008882 ) ) ;
#346 = ORIENTED_EDGE ( 'NONE', *, *, #8932, .T. ) ;
#347 =( GEOMETRIC_REPRESENTATION_CONTEXT ( 3 ) GLOBAL_UNCERTAINTY_ASSIGNED_CONTEXT ( ( #4745 ) ) GLOBAL_UNIT_ASSIGNED_CONTEXT ( ( #17997, #14301, #12516 ) ) REPRESENTATION_CONTEXT ( 'NONE', 'WORKASPACE' ) );
#348 = DIRECTION ( 'NONE',  ( 0.000000000000000000, 1.000000000000000000, -0.000000000000000000 ) ) ;
#349 = VECTOR ( 'NONE', #3642, 1000.000000000000000 ) ;
#350 = CARTESIAN_POINT ( 'NONE',  ( -2.828427124746189403, 2.828427124746190291, 12.87500000000001066 ) ) ;
#351 = DIRECTION ( 'NONE',  ( 0.000000000000000000, 0.000000000000000000, 1.000000000000000000 ) ) ;
#352 = CARTESIAN_POINT ( 'NONE',  ( 2.149474931388133836, 6.264553569211843254, -3.644669744206378681 ) ) ;
#353 = PLANE ( 'NONE',  #2572 ) ;
#354 = CARTESIAN_POINT ( 'NONE',  ( 69.75000000109245946, 11.46158073645647235, 16.46158073645647235 ) ) ;
#355 = AXIS2_PLACEMENT_3D ( 'NONE', #12842, #20101, #14526 ) ;
#356 = ORIENTED_EDGE ( 'NONE', *, *, #112, .T. ) ;
#357 = VECTOR ( 'NONE', #88, 1000.000000000000114 ) ;
#358 = CARTESIAN_POINT ( 'NONE',  ( -90.00000000000000000, 0.000000000000000000, 0.000000000000000000 ) ) ;
#359 = CARTESIAN_POINT ( 'NONE',  ( 0.000000000000000000, 0.000000000000000000, 0.000000000000000000 ) ) ;
#360 = CARTESIAN_POINT ( 'NONE',  ( 65.75000000109247367, 8.538419263543522320, 16.46158073645647235 ) ) ;
#361 = CARTESIAN_POINT ( 'NONE',  ( 1.025207404391860050E-15, 3.458734125000000326, 17.18750000136560274 ) ) ;
#362 = DIRECTION ( 'NONE',  ( -0.000000000000000000, -1.000000000000000000, -0.000000000000000000 ) ) ;
#363 = CARTESIAN_POINT ( 'NONE',  ( -2.445694354108820523, 2.445694354108820523, -2.137499998634403653 ) ) ;
#364 = AXIS2_PLACEMENT_3D ( 'NONE', #4231, #22417, #9754 ) ;
#365 = CARTESIAN_POINT ( 'NONE',  ( 4.000000000000000000, 1.656854249492381248, 1.862500000000001599 ) ) ;
#366 = CARTESIAN_POINT ( 'NONE',  ( -71.30000000218494449, 8.232233047033629347, 13.23223304703362402 ) ) ;
#367 = CARTESIAN_POINT ( 'NONE',  ( -2.445694354108819191, 2.445694354108820523, 15.31250000136560452 ) ) ;
#368 = CYLINDRICAL_SURFACE ( 'NONE', #9, 8.749000000000002331 ) ;
#369 = EDGE_LOOP ( 'NONE', ( #10172, #18701, #9343, #9622 ) ) ;
#370 = CARTESIAN_POINT ( 'NONE',  ( -68.10000000109248219, 9.143825827087049163, 17.06698730000000097 ) ) ;
#371 = ORIENTED_EDGE ( 'NONE', *, *, #16704, .T. ) ;
#372 = CARTESIAN_POINT ( 'NONE',  ( 57.18750000000000000, 9.999999999999978684, 10.99999999999999645 ) ) ;
#373 = CARTESIAN_POINT ( 'NONE',  ( -71.90000000109246514, 10.85617417291294551, 12.93301269999999370 ) ) ;
#374 = SHAPE_DEFINITION_REPRESENTATION ( #9332, #13579 ) ;
#375 = VERTEX_POINT ( 'NONE', #16712 ) ;
#376 = CARTESIAN_POINT ( 'NONE',  ( -2.828427124746190291, 2.828427124746190291, 1.300000002731187543 ) ) ;
#377 = ORIENTED_EDGE ( 'NONE', *, *, #743, .F. ) ;
#378 = VECTOR ( 'NONE', #16810, 1000.000000000000114 ) ;
#379 = VECTOR ( 'NONE', #18858, 1000.000000000000000 ) ;
#380 = ORIENTED_EDGE ( 'NONE', *, *, #8945, .F. ) ;
#381 = CARTESIAN_POINT ( 'NONE',  ( 1.432654583217641386, 3.458734125000000770, 15.37500000136560807 ) ) ;
#382 = CARTESIAN_POINT ( 'NONE',  ( 53.43750000000000711, 10.00000000000000711, 17.99999999999999645 ) ) ;
#383 = VECTOR ( 'NONE', #917, 1000.000000000000000 ) ;
#384 = CARTESIAN_POINT ( 'NONE',  ( -67.50000000109247367, 7.933012699999995476, 14.14382582708705094 ) ) ;
#385 = AXIS2_PLACEMENT_3D ( 'NONE', #6028, #512, #265 ) ;
#386 = CARTESIAN_POINT ( 'NONE',  ( 70.20000000109246230, 12.06698729999999919, 14.14382582708705094 ) ) ;
#387 = ADVANCED_FACE ( 'NONE', ( #290 ), #419, .F. ) ;
#388 = CARTESIAN_POINT ( 'NONE',  ( -67.75000000109245946, 8.538419263543524096, 13.53841926354352054 ) ) ;
#389 = CARTESIAN_POINT ( 'NONE',  ( 2.445694354108822299, -2.445694354108820079, 12.06250000136560629 ) ) ;
#390 = CARTESIAN_POINT ( 'NONE',  ( 18.14354716966726144, -11.25000000000000355, 10.00000000000008882 ) ) ;
#391 = CARTESIAN_POINT ( 'NONE',  ( 55.65393183416158251, 6.971812294485357775, 16.17458954617365663 ) ) ;
#392 = CARTESIAN_POINT ( 'NONE',  ( -9.000000000000000000, 1.102182119232617714E-15, 1.102182119232617714E-15 ) ) ;
#393 = CARTESIAN_POINT ( 'NONE',  ( 55.21875000000000000, 13.00000000000000711, 16.24264068711927322 ) ) ;
#394 = CARTESIAN_POINT ( 'NONE',  ( 6.625378842019205905, 0.6908453745559488546, 10.00000000000008882 ) ) ;
#395 = CARTESIAN_POINT ( 'NONE',  ( -3.999999999999999112, 0.000000000000000000, 17.12500000273119838 ) ) ;
#396 = EDGE_CURVE ( 'NONE', #2255, #17303, #7746, .T. ) ;
#397 = DIRECTION ( 'NONE',  ( -1.848892746611742040E-32, -0.3420201433256690460, 0.9396926207859083169 ) ) ;
#398 = AXIS2_PLACEMENT_3D ( 'NONE', #11529, #8386, #10076 ) ;
#399 = ORIENTED_EDGE ( 'NONE', *, *, #10605, .F. ) ;
#400 = CARTESIAN_POINT ( 'NONE',  ( 70.39999999999999147, 8.232233047033629347, 13.23223304703362402 ) ) ;
#401 = CARTESIAN_POINT ( 'NONE',  ( 1.519999999999999574, 0.000000000000000000, -6.760799999999997034 ) ) ;
#402 = VERTEX_POINT ( 'NONE', #20872 ) ;
#403 = CARTESIAN_POINT ( 'NONE',  ( 56.31018183416157541, 12.99999999999999822, 15.06805114094562192 ) ) ;
#405 = COLOUR_RGB ( '', 0.66274510, 0.83137255, 0.94901961) ;
#404 = APPLICATION_PROTOCOL_DEFINITION ( 'draft international standard', 'automotive_design', 1998, #10237 ) ;
#406 = CARTESIAN_POINT ( 'NONE',  ( 4.000000000000000000, 1.656854249492381248, -2.012499997268811569 ) ) ;
#407 = DIRECTION ( 'NONE',  ( 0.000000000000000000, 0.000000000000000000, -1.000000000000000000 ) ) ;
#408 = ORIENTED_EDGE ( 'NONE', *, *, #13246, .T. ) ;
#409 = CARTESIAN_POINT ( 'NONE',  ( 4.000000000000001776, -1.656854249492379694, 12.43750000000001066 ) ) ;
#410 = DIRECTION ( 'NONE',  ( -1.000000000000000000, 0.000000000000000000, -0.000000000000000000 ) ) ;
#411 = DIRECTION ( 'NONE',  ( 0.000000000000000000, 0.000000000000000000, -1.000000000000000000 ) ) ;
#412 = ORIENTED_EDGE ( 'NONE', *, *, #302, .T. ) ;
#413 = CARTESIAN_POINT ( 'NONE',  ( -70.80000000218494449, 12.50000000000000000, 14.99999999999999645 ) ) ;
#414 = CARTESIAN_POINT ( 'NONE',  ( -3.458734125000000326, -1.432654583217642497, 1.050000001365596791 ) ) ;
#415 = AXIS2_PLACEMENT_3D ( 'NONE', #22234, #2115, #9450 ) ;
#416 = ADVANCED_FACE ( 'NONE', ( #532 ), #16955, .F. ) ;
#417 = CARTESIAN_POINT ( 'NONE',  ( 69.49999999999998579, 7.499999999999996447, 14.99999999999999645 ) ) ;
#418 = ADVANCED_FACE ( 'NONE', ( #22570 ), #11946, .T. ) ;
#419 = CYLINDRICAL_SURFACE ( 'NONE', #6270, 2.500000000000007550 ) ;
#420 = DIRECTION ( 'NONE',  ( 1.000000000000000000, 0.000000000000000000, 0.000000000000000000 ) ) ;
#421 = CARTESIAN_POINT ( 'NONE',  ( 54.97106816583843880, 5.971812294485345340, 13.41119689145326710 ) ) ;
#422 = CARTESIAN_POINT ( 'NONE',  ( -2.445694354108819635, -2.445694354108820523, -2.137499998634403653 ) ) ;
#423 = CARTESIAN_POINT ( 'NONE',  ( -1.432654583217639832, -3.458734125000000326, 14.87500000136560807 ) ) ;
#424 = EDGE_CURVE ( 'NONE', #2869, #9385, #10142, .T. ) ;
#425 = DIRECTION ( 'NONE',  ( 0.000000000000000000, 0.7071067811865414665, -0.7071067811865536790 ) ) ;
#426 = CARTESIAN_POINT ( 'NONE',  ( -71.30000000109247082, 12.06698729999999919, 15.85617417291294196 ) ) ;
#427 = CARTESIAN_POINT ( 'NONE',  ( 2.828427124746191179, 2.828427124746190291, 16.62500000000001066 ) ) ;
#428 = VERTEX_POINT ( 'NONE', #15531 ) ;
#429 = CARTESIAN_POINT ( 'NONE',  ( -2.828427124746188515, -2.828427124746190735, 14.12500000000001066 ) ) ;
#430 = DIRECTION ( 'NONE',  ( 0.000000000000000000, 0.000000000000000000, -1.000000000000000000 ) ) ;
#431 = CARTESIAN_POINT ( 'NONE',  ( -71.35000000109246798, 8.538419263543522320, 16.46158073645647235 ) ) ;
#432 = ORIENTED_EDGE ( 'NONE', *, *, #13078, .F. ) ;
#433 = VERTEX_POINT ( 'NONE', #17433 ) ;
#434 = SURFACE_STYLE_FILL_AREA ( #309 ) ;
#435 = DIRECTION ( 'NONE',  ( -0.9396926207859107594, -0.3420201433256623291, 1.540743955509804830E-32 ) ) ;
#436 = ORIENTED_EDGE ( 'NONE', *, *, #2367, .T. ) ;
#437 = DIRECTION ( 'NONE',  ( 1.000000000000000000, 7.703719777548943412E-32, 0.000000000000000000 ) ) ;
#438 = VERTEX_POINT ( 'NONE', #2331 ) ;
#439 = PRODUCT_DEFINITION_CONTEXT ( 'detailed design', #1495, 'design' ) ;
#440 = CARTESIAN_POINT ( 'NONE',  ( 56.75231816583843170, 7.219692298483957771, 17.87654654797633924 ) ) ;
#441 = EDGE_CURVE ( 'NONE', #4290, #23005, #13728, .T. ) ;
#442 = CARTESIAN_POINT ( 'NONE',  ( 71.20000000109246230, 10.85617417291294551, 17.06698729999999742 ) ) ;
#443 = CARTESIAN_POINT ( 'NONE',  ( 0.000000000000000000, 6.478011392632890164, 6.807171995660607600 ) ) ;
#444 = CARTESIAN_POINT ( 'NONE',  ( 70.85000000109246798, 7.933012699999995476, 14.99999999999999645 ) ) ;
#445 = EDGE_CURVE ( 'NONE', #15027, #12453, #14670, .T. ) ;
#446 = ORIENTED_EDGE ( 'NONE', *, *, #4266, .T. ) ;
#447 = CARTESIAN_POINT ( 'NONE',  ( -1.656854249492380138, -3.999999999999999112, 13.31250000273119660 ) ) ;
#448 = CARTESIAN_POINT ( 'NONE',  ( -69.70000000000000284, 9.999999999999998224, 12.49999999999999289 ) ) ;
#449 = ADVANCED_BREP_SHAPE_REPRESENTATION ( '', ( #22288, #7318 ), #28 ) ;
#450 = CARTESIAN_POINT ( 'NONE',  ( 52.18518183416157541, 10.06805114094561659, 10.99999999999999645 ) ) ;
#451 = CARTESIAN_POINT ( 'NONE',  ( -1.647987302177966740E-14, -7.505553499465137612, -3.119443416399232394 ) ) ;
#452 = EDGE_CURVE ( 'NONE', #2752, #12712, #14700, .T. ) ;
#453 = CYLINDRICAL_SURFACE ( 'NONE', #16618, 4.000000000000001776 ) ;
#454 = DIRECTION ( 'NONE',  ( 0.06805114094563399774, -0.7054675904022866817, -0.7054675904022729149 ) ) ;
#455 = EDGE_CURVE ( 'NONE', #7307, #20911, #18012, .T. ) ;
#456 = CARTESIAN_POINT ( 'NONE',  ( -67.00000000109245946, 9.143825827087052716, 12.93301269999999192 ) ) ;
#457 = CARTESIAN_POINT ( 'NONE',  ( 4.204115023516791005, -1.660442669500199919, -3.602151381774560068 ) ) ;
#458 = EDGE_LOOP ( 'NONE', ( #20331, #17949, #19339, #14429 ) ) ;
#459 = CARTESIAN_POINT ( 'NONE',  ( -4.000000000000000000, 2.511478553582031203, -3.469254451724764543 ) ) ;
#460 = DIRECTION ( 'NONE',  ( -7.087422195345011518E-32, -1.000000000000000000, -0.000000000000000000 ) ) ;
#461 = B_SPLINE_CURVE_WITH_KNOTS ( 'NONE', 3,
 ( #13230, #10227, #23012, #13936, #854, #2656 ),
 .UNSPECIFIED., .F., .F.,
 ( 4, 2, 4 ),
 ( 0.006695446894088488872, 0.008593684019695166376, 0.01049192114530184475 ),
 .UNSPECIFIED. ) ;
#462 = VERTEX_POINT ( 'NONE', #5930 ) ;
#463 = CARTESIAN_POINT ( 'NONE',  ( 54.99999999999992895, 15.00000000000000000, 1.836970198721037478E-15 ) ) ;
#464 = DIRECTION ( 'NONE',  ( 0.000000000000000000, 0.000000000000000000, 1.000000000000000000 ) ) ;
#465 = CARTESIAN_POINT ( 'NONE',  ( 9.000000000000000000, 0.000000000000000000, -4.000000000000000888 ) ) ;
#466 = DIRECTION ( 'NONE',  ( -1.000000000000000000, 0.000000000000000000, 1.224646799147353207E-16 ) ) ;
#467 = ORIENTED_EDGE ( 'NONE', *, *, #9823, .T. ) ;
#468 = CARTESIAN_POINT ( 'NONE',  ( 72.50000000000000000, 9.999999999999998224, 14.99999999999999645 ) ) ;
#469 = ORIENTED_EDGE ( 'NONE', *, *, #19443, .T. ) ;
#470 = LINE ( 'NONE', #15224, #23263 ) ;
#471 = CARTESIAN_POINT ( 'NONE',  ( -2.828427124746189403, 2.828427124746190291, 13.87500000000001066 ) ) ;
#472 = LINE ( 'NONE', #5983, #26 ) ;
#473 = DIRECTION ( 'NONE',  ( 0.000000000000000000, 1.224646799147353207E-16, 1.000000000000000000 ) ) ;
#474 =( NAMED_UNIT ( * ) PLANE_ANGLE_UNIT ( ) SI_UNIT ( $, .RADIAN. ) );
#475 = CARTESIAN_POINT ( 'NONE',  ( 70.65000000109246514, 9.999999999999998224, 17.06698730000000097 ) ) ;
#476 = VERTEX_POINT ( 'NONE', #7853 ) ;
#477 = CARTESIAN_POINT ( 'NONE',  ( 5.000000000000000888, 5.400000000000000355, -1.000000000000000000 ) ) ;
#478 = DIRECTION ( 'NONE',  ( 0.000000000000000000, 0.000000000000000000, 1.000000000000000000 ) ) ;
#479 = EDGE_CURVE ( 'NONE', #2500, #428, #11820, .T. ) ;
#480 = CIRCLE ( 'NONE', #8921, 0.03079999999999836341 ) ;
#481 = CARTESIAN_POINT ( 'NONE',  ( 71.55000000109245661, 8.538419263543522320, 16.46158073645647235 ) ) ;
#482 = CARTESIAN_POINT ( 'NONE',  ( 3.458734125000001214, 1.432654583217640498, 14.00000000136560629 ) ) ;
#483 = CARTESIAN_POINT ( 'NONE',  ( 35.28529930323381336, -9.000000000000001776, 10.00000000000008882 ) ) ;
#484 = EDGE_CURVE ( 'NONE', #12003, #2520, #19247, .T. ) ;
#485 = CARTESIAN_POINT ( 'NONE',  ( -2.445694354108819635, -2.445694354108820967, -0.8874999986344025427 ) ) ;
#486 = CARTESIAN_POINT ( 'NONE',  ( 4.000000000000000000, 4.898587196589412829E-16, 0.8000000000000020428 ) ) ;
#487 = LINE ( 'NONE', #7810, #20366 ) ;
#488 = CARTESIAN_POINT ( 'NONE',  ( 2.445694354108821855, -2.445694354108820079, 13.81250000136560629 ) ) ;
#489 = DIRECTION ( 'NONE',  ( -1.000000000000000000, -0.000000000000000000, -0.000000000000000000 ) ) ;
#490 = ORIENTED_EDGE ( 'NONE', *, *, #671, .F. ) ;
#491 = CARTESIAN_POINT ( 'NONE',  ( -2.828427124746189403, 2.828427124746190291, 16.00000000273119838 ) ) ;
#492 = ORIENTED_EDGE ( 'NONE', *, *, #19288, .T. ) ;
#493 = CARTESIAN_POINT ( 'NONE',  ( 58.68750000000000000, 9.999999999999978684, 10.99999999999999645 ) ) ;
#494 = CARTESIAN_POINT ( 'NONE',  ( -71.70000000109247651, 7.933012699999995476, 14.14382582708705094 ) ) ;
#495 = APPLICATION_PROTOCOL_DEFINITION ( 'draft international standard', 'automotive_design', 1998, #17102 ) ;
#496 = ORIENTED_EDGE ( 'NONE', *, *, #9040, .T. ) ;
#497 = CARTESIAN_POINT ( 'NONE',  ( -19.99999999999999645, -9.000000000000003553, 5.000000000000079936 ) ) ;
#498 = ORIENTED_EDGE ( 'NONE', *, *, #23535, .T. ) ;
#499 = ORIENTED_EDGE ( 'NONE', *, *, #310, .T. ) ;
#500 = CARTESIAN_POINT ( 'NONE',  ( 1.432654583217643163, -3.458734124999999882, 15.00000000136560629 ) ) ;
#501 = CARTESIAN_POINT ( 'NONE',  ( 55.12500000000000711, 12.12132034355964727, 17.12132034355963484 ) ) ;
#502 = AXIS2_PLACEMENT_3D ( 'NONE', #19793, #15651, #23149 ) ;
#503 = CARTESIAN_POINT ( 'NONE',  ( -66.95000000109246230, 11.46158073645647235, 13.53841926354352232 ) ) ;
#504 = AXIS2_PLACEMENT_3D ( 'NONE', #17379, #9846, #2632 ) ;
#505 = CARTESIAN_POINT ( 'NONE',  ( 70.55000000109247082, 8.538419263543522320, 16.46158073645647235 ) ) ;
#506 = CARTESIAN_POINT ( 'NONE',  ( -67.35000000109246798, 11.46158073645647235, 16.46158073645647235 ) ) ;
#507 = CARTESIAN_POINT ( 'NONE',  ( -19.55556463033274284, -11.25000000000000355, 5.000000000000079936 ) ) ;
#508 = CARTESIAN_POINT ( 'NONE',  ( 56.31018183416157541, 12.99999999999999822, 15.06805114094562192 ) ) ;
#509 = CARTESIAN_POINT ( 'NONE',  ( -2.445694354108820523, 2.445694354108820523, 2.862500001365597235 ) ) ;
#510 = CARTESIAN_POINT ( 'NONE',  ( -2.445694354108819191, 2.445694354108820523, 10.31250000136560629 ) ) ;
#511 = CARTESIAN_POINT ( 'NONE',  ( 1.971781867644420635E-15, -4.000000000000000000, 14.37500000273119660 ) ) ;
#512 = DIRECTION ( 'NONE',  ( -1.224646799147353207E-16, 0.000000000000000000, -1.000000000000000000 ) ) ;
#513 = AXIS2_PLACEMENT_3D ( 'NONE', #21958, #21850, #9422 ) ;
#514 = ORIENTED_EDGE ( 'NONE', *, *, #14781, .F. ) ;
#515 = CARTESIAN_POINT ( 'NONE',  ( 72.09999999999999432, 9.999999999999998224, 12.49999999999999289 ) ) ;
#516 = EDGE_LOOP ( 'NONE', ( #68, #21518, #3055, #2681, #12780, #20192, #1158, #14031, #18308, #16919, #16791, #2387, #4988, #13331, #13453, #17105, #21865, #10269, #6716 ) ) ;
#517 = CARTESIAN_POINT ( 'NONE',  ( 55.74768183416157541, 7.830560233210222876, 17.07320092032950498 ) ) ;
#518 = PRESENTATION_STYLE_ASSIGNMENT (( #3876 ) ) ;
#519 = CARTESIAN_POINT ( 'NONE',  ( 3.458734125000000326, 4.235727675282971730E-16, 2.237500001365596791 ) ) ;
#521 = AXIS2_PLACEMENT_3D ( 'NONE', #5030, #23463, #14389 ) ;
#520 = PRODUCT_DEFINITION ( 'UNKNOWN', '', #22130, #7875 ) ;
#522 = ORIENTED_EDGE ( 'NONE', *, *, #19880, .T. ) ;
#523 = CARTESIAN_POINT ( 'NONE',  ( 1.656854249492384135, -3.999999999999999112, 12.31250000000001243 ) ) ;
#524 = EDGE_CURVE ( 'NONE', #14801, #21630, #9665, .T. ) ;
#525 = LINE ( 'NONE', #869, #679 ) ;
#526 = PLANE ( 'NONE',  #15257 ) ;
#527 = ORIENTED_EDGE ( 'NONE', *, *, #17288, .T. ) ;
#528 = CARTESIAN_POINT ( 'NONE',  ( -69.50000000218494733, 8.232233047033627571, 16.76776695296636532 ) ) ;
#529 = FACE_OUTER_BOUND ( 'NONE', #22717, .T. ) ;
#530 = CARTESIAN_POINT ( 'NONE',  ( -3.525817189091416282, -5.469921996229804684, -3.700000000000000622 ) ) ;
#531 = CARTESIAN_POINT ( 'NONE',  ( 68.34999999999999432, 12.50000000000000000, 16.03553390593273420 ) ) ;
#532 = FACE_OUTER_BOUND ( 'NONE', #9949, .T. ) ;
#533 = DIRECTION ( 'NONE',  ( 0.000000000000000000, 0.000000000000000000, 1.000000000000000000 ) ) ;
#534 = CARTESIAN_POINT ( 'NONE',  ( 56.47106816583845301, 6.971812294485350670, 13.82541045382635403 ) ) ;
#535 = CARTESIAN_POINT ( 'NONE',  ( -1.432654583217641164, -3.458734125000000326, 4.175000001365593683 ) ) ;
#536 = CARTESIAN_POINT ( 'NONE',  ( -1.432654583217639166, 3.458734125000000770, 16.50000000136560629 ) ) ;
#537 = DIRECTION ( 'NONE',  ( 1.000000000000000000, -0.000000000000000000, -0.000000000000000000 ) ) ;
#538 = DIRECTION ( 'NONE',  ( -1.000000000000000000, -0.000000000000000000, 0.000000000000000000 ) ) ;
#539 = ORIENTED_EDGE ( 'NONE', *, *, #10100, .T. ) ;
#540 = CARTESIAN_POINT ( 'NONE',  ( -0.5276280594146446346, 4.314175951381965746, -3.320322319201721495 ) ) ;
#541 =( BOUNDED_CURVE ( )  B_SPLINE_CURVE ( 2, ( #16400, #7064, #18073, #8877, #7426, #5378, #16170, #18188, #11021 ),
 .UNSPECIFIED., .F., .F. ) 
 B_SPLINE_CURVE_WITH_KNOTS ( ( 3, 2, 2, 2, 3 ),
 ( 0.4999999999999991118, 0.5156249999999995559, 0.5312500000000000000, 0.5468750000000004441, 0.5625000000000008882 ),
 .UNSPECIFIED. ) 
 CURVE ( )  GEOMETRIC_REPRESENTATION_ITEM ( )  RATIONAL_B_SPLINE_CURVE ( ( 1.000000000000004219, 0.9238795325112824086, 1.000000000000000000, 0.9238795325112867385, 1.000000000000000000, 0.9238795325112867385, 1.000000000000000000, 0.9238795325112824086, 1.000000000000004219 ) ) 
 REPRESENTATION_ITEM ( '' )  );
#542 = CARTESIAN_POINT ( 'NONE',  ( 1.656854249492380360, 4.000000000000000000, 5.112500002731189319 ) ) ;
#543 = CARTESIAN_POINT ( 'NONE',  ( -70.85000000109246798, 9.999999999999998224, 12.93301269999999192 ) ) ;
#544 = ORIENTED_EDGE ( 'NONE', *, *, #4528, .T. ) ;
#545 = ORIENTED_EDGE ( 'NONE', *, *, #18329, .F. ) ;
#546 = EDGE_CURVE ( 'NONE', #10073, #7680, #4255, .T. ) ;
#547 = EDGE_CURVE ( 'NONE', #15019, #16065, #20991, .T. ) ;
#548 = FACE_OUTER_BOUND ( 'NONE', #8173, .T. ) ;
#549 = VERTEX_POINT ( 'NONE', #15298 ) ;
#550 = CARTESIAN_POINT ( 'NONE',  ( 3.522875095019493141, -2.820352903225631369, -3.598441714920572299 ) ) ;
#551 = EDGE_CURVE ( 'NONE', #19948, #10458, #10853, .T. ) ;
#552 = CARTESIAN_POINT ( 'NONE',  ( 66.35000000218495586, 7.499999999999995559, 16.03553390593273420 ) ) ;
#553 = CIRCLE ( 'NONE', #17789, 4.000000000000001776 ) ;
#554 = CARTESIAN_POINT ( 'NONE',  ( 4.000000000000000888, 4.898587196589412829E-16, 19.50000000000001066 ) ) ;
#555 = CARTESIAN_POINT ( 'NONE',  ( 71.30000000109247082, 12.06698730000000275, 15.85617417291294196 ) ) ;
#556 = CIRCLE ( 'NONE', #10551, 4.000000000000000000 ) ;
#557 = ORIENTED_EDGE ( 'NONE', *, *, #22228, .T. ) ;
#558 = CARTESIAN_POINT ( 'NONE',  ( 2.828427124746191179, 2.828427124746190291, 13.75000000273119483 ) ) ;
#559 = DIRECTION ( 'NONE',  ( 0.000000000000000000, 0.000000000000000000, 1.000000000000000000 ) ) ;
#560 = CARTESIAN_POINT ( 'NONE',  ( 53.40393183416157541, 14.02818770551463956, 13.41119689145323335 ) ) ;
#561 = DIRECTION ( 'NONE',  ( -1.000000000000000000, -7.703719777548943412E-32, 0.000000000000000000 ) ) ;
#562 = CARTESIAN_POINT ( 'NONE',  ( 3.458734125000001214, 1.432654583217640498, 19.00000000136560629 ) ) ;
#563 = LINE ( 'NONE', #5844, #11693 ) ;
#564 = LINE ( 'NONE', #7663, #15899 ) ;
#565 = EDGE_LOOP ( 'NONE', ( #20115, #18574, #6373, #5474, #16669 ) ) ;
#566 = CARTESIAN_POINT ( 'NONE',  ( 1.600000000000004086, 8.247996192257451316E-16, 6.735000000000022524 ) ) ;
#567 = ORIENTED_EDGE ( 'NONE', *, *, #3730, .T. ) ;
#568 = CARTESIAN_POINT ( 'NONE',  ( 52.68750000000000711, 9.999999999999989342, 11.99999999999999467 ) ) ;
#569 = DIRECTION ( 'NONE',  ( -1.000000000000000000, 0.000000000000000000, 0.000000000000000000 ) ) ;
#570 = ORIENTED_EDGE ( 'NONE', *, *, #15740, .T. ) ;
#571 = DIRECTION ( 'NONE',  ( -1.000000000000000000, -0.000000000000000000, 0.000000000000000000 ) ) ;
#572 = DIRECTION ( 'NONE',  ( 0.000000000000000000, 0.000000000000000000, -1.000000000000000000 ) ) ;
#573 = CARTESIAN_POINT ( 'NONE',  ( 0.000000000000000000, -3.174628368996134320, 8.152713396088753228 ) ) ;
#574 = ADVANCED_FACE ( 'NONE', ( #17777 ), #21577, .F. ) ;
#575 = AXIS2_PLACEMENT_3D ( 'NONE', #18890, #2475, #16877 ) ;
#576 = DIRECTION ( 'NONE',  ( 0.3420201433256622181, 0.9396926207859107594, -6.162975822039141593E-32 ) ) ;
#577 = ORIENTED_EDGE ( 'NONE', *, *, #10412, .F. ) ;
#578 = CARTESIAN_POINT ( 'NONE',  ( -1.600000000000004086, 1.012170579495290078E-15, 8.265000000000021885 ) ) ;
#579 = ORIENTED_EDGE ( 'NONE', *, *, #15797, .F. ) ;
#580 =( BOUNDED_CURVE ( )  B_SPLINE_CURVE ( 2, ( #16295, #1659, #8523, #12481, #6712, #3467, #17625, #14148, #21414 ),
 .UNSPECIFIED., .F., .F. ) 
 B_SPLINE_CURVE_WITH_KNOTS ( ( 3, 2, 2, 2, 3 ),
 ( 0.4500000000000000111, 0.4625000000000000222, 0.4749999999999999778, 0.4874999999999999889, 0.5000000000000000000 ),
 .UNSPECIFIED. ) 
 CURVE ( )  GEOMETRIC_REPRESENTATION_ITEM ( )  RATIONAL_B_SPLINE_CURVE ( ( 1.000000000000000000, 0.9238795325112867385, 1.000000000000000000, 0.9238795325112867385, 1.000000000000000000, 0.9238795325112867385, 1.000000000000000000, 0.9238795325112867385, 1.000000000000000000 ) ) 
 REPRESENTATION_ITEM ( '' )  );
#581 = DIRECTION ( 'NONE',  ( 0.000000000000000000, 0.000000000000000000, -1.000000000000000000 ) ) ;
#582 = CARTESIAN_POINT ( 'NONE',  ( 4.000000000000000888, 4.898587196589412829E-16, 13.50000000000001066 ) ) ;
#583 = ADVANCED_FACE ( 'NONE', ( #22922 ), #6649, .T. ) ;
#584 = FACE_OUTER_BOUND ( 'NONE', #22626, .T. ) ;
#585 = EDGE_CURVE ( 'NONE', #18482, #8738, #4962, .T. ) ;
#586 = CARTESIAN_POINT ( 'NONE',  ( 118.3095189484530181, -10.00000000000001599, 34.11836509645782201 ) ) ;
#587 = CARTESIAN_POINT ( 'NONE',  ( 27.50000000000000000, 4.500000000000001776, -36.31025403784445871 ) ) ;
#588 = CARTESIAN_POINT ( 'NONE',  ( 69.45000000109247651, 9.999999999999998224, 12.93301269999999192 ) ) ;
#589 = VERTEX_POINT ( 'NONE', #18015 ) ;
#590 = VECTOR ( 'NONE', #2193, 1000.000000000000000 ) ;
#591 = DIRECTION ( 'NONE',  ( -1.000000000000000000, 0.000000000000000000, 0.000000000000000000 ) ) ;
#592 = VECTOR ( 'NONE', #4754, 1000.000000000000000 ) ;
#593 = CARTESIAN_POINT ( 'NONE',  ( 72.15000000109246514, 11.46158073645647235, 16.46158073645647235 ) ) ;
#594 = CARTESIAN_POINT ( 'NONE',  ( 1.432654583217641164, 3.458734125000000326, 13.12500000136560274 ) ) ;
#595 = DIRECTION ( 'NONE',  ( 0.3420201433256622181, 0.9396926207859107594, -6.162975822039141593E-32 ) ) ;
#596 = CARTESIAN_POINT ( 'NONE',  ( 32.14370665323380649, -9.000000000000003553, 5.000000000000079936 ) ) ;
#597 = CARTESIAN_POINT ( 'NONE',  ( 1.656854249492380360, 4.000000000000000000, 1.987500000000001599 ) ) ;
#598 = CARTESIAN_POINT ( 'NONE',  ( -3.999999999999999112, 1.656854249492380582, 12.93750000000001066 ) ) ;
#599 = CARTESIAN_POINT ( 'NONE',  ( 44.71007725323381976, -9.000000000000003553, 5.000000000000079936 ) ) ;
#600 = LINE ( 'NONE', #1067, #16099 ) ;
#601 = VECTOR ( 'NONE', #9815, 1000.000000000000000 ) ;
#602 = ORIENTED_EDGE ( 'NONE', *, *, #19154, .T. ) ;
#603 = CARTESIAN_POINT ( 'NONE',  ( -66.70000000109246230, 7.933012699999995476, 14.14382582708705094 ) ) ;
#604 = EDGE_LOOP ( 'NONE', ( #19723, #19052, #12371, #5086 ) ) ;
#605 = CARTESIAN_POINT ( 'NONE',  ( 57.37500000000000000, 7.171572875253794166, 12.17157287525381726 ) ) ;
#606 = CARTESIAN_POINT ( 'NONE',  ( -67.85000000109246798, 9.999999999999998224, 12.93301269999999192 ) ) ;
#607 = APPLICATION_PROTOCOL_DEFINITION ( 'draft international standard', 'automotive_design', 1998, #8871 ) ;
#608 = ADVANCED_FACE ( 'NONE', ( #8331 ), #21063, .T. ) ;
#609 = ORIENTED_EDGE ( 'NONE', *, *, #1017, .T. ) ;
#610 = CARTESIAN_POINT ( 'NONE',  ( 4.999999999999999112, -5.538577986808850717, -6.772677083992447500 ) ) ;
#611 = VERTEX_POINT ( 'NONE', #2056 ) ;
#612 = ADVANCED_FACE ( 'NONE', ( #9398 ), #13898, .F. ) ;
#613 = ORIENTED_EDGE ( 'NONE', *, *, #10738, .T. ) ;
#614 = CARTESIAN_POINT ( 'NONE',  ( 1.025207404391860050E-15, 3.458734125000000770, 18.43750000136560629 ) ) ;
#615 = EDGE_CURVE ( 'NONE', #9363, #5525, #3178, .T. ) ;
#616 = CARTESIAN_POINT ( 'NONE',  ( 58.50000000000000000, 12.12132034355963484, 12.87867965644034740 ) ) ;
#617 = ADVANCED_FACE ( 'NONE', ( #10330 ), #17840, .T. ) ;
#618 = CARTESIAN_POINT ( 'NONE',  ( -67.35000000109248219, 8.538419263543522320, 16.46158073645647235 ) ) ;
#619 = CARTESIAN_POINT ( 'NONE',  ( 68.90000000109247935, 9.143825827087049163, 17.06698730000000097 ) ) ;
#620 = CARTESIAN_POINT ( 'NONE',  ( -72.29999999999998295, 12.50000000000000000, 14.99999999999999645 ) ) ;
#621 = DIRECTION ( 'NONE',  ( -0.000000000000000000, -1.000000000000000000, -0.000000000000000000 ) ) ;
#622 = CARTESIAN_POINT ( 'NONE',  ( 54.15393183416158251, 6.971812294485357775, 16.17458954617365663 ) ) ;
#623 = CARTESIAN_POINT ( 'NONE',  ( 2.000000000000001776, 0.000000000000000000, 0.000000000000000000 ) ) ;
#624 = CARTESIAN_POINT ( 'NONE',  ( -2.117863837641485618E-16, 3.458734125000000770, 4.737500001365595459 ) ) ;
#625 = CARTESIAN_POINT ( 'NONE',  ( 2.445694354108821855, -2.445694354108820079, 10.81250000136560452 ) ) ;
#626 = CARTESIAN_POINT ( 'NONE',  ( 2.828427124746191179, 2.828427124746190291, 11.75000000273119660 ) ) ;
#627 = ORIENTED_EDGE ( 'NONE', *, *, #11500, .T. ) ;
#628 = FACE_OUTER_BOUND ( 'NONE', #9210, .T. ) ;
#629 = ORIENTED_EDGE ( 'NONE', *, *, #21485, .F. ) ;
#630 = CARTESIAN_POINT ( 'NONE',  ( 59.87268183416157541, 7.926799079670491466, 12.83056023321021755 ) ) ;
#631 = CARTESIAN_POINT ( 'NONE',  ( 6.353591512924457348E-16, -3.458734125000000326, 1.987500001365596569 ) ) ;
#632 = DIRECTION ( 'NONE',  ( 1.000000000000000000, 0.000000000000000000, 0.000000000000000000 ) ) ;
#633 = VERTEX_POINT ( 'NONE', #17729 ) ;
#634 = CARTESIAN_POINT ( 'NONE',  ( 2.828427124746192067, -2.828427124746189847, 11.37500000000001066 ) ) ;
#635 = LINE ( 'NONE', #22428, #20559 ) ;
#636 = EDGE_CURVE ( 'NONE', #21119, #17601, #4711, .T. ) ;
#637 = DIRECTION ( 'NONE',  ( -0.000000000000000000, -0.000000000000000000, 1.000000000000000000 ) ) ;
#638 = ORIENTED_EDGE ( 'NONE', *, *, #18988, .T. ) ;
#639 = EDGE_CURVE ( 'NONE', #6641, #11647, #14022, .T. ) ;
#640 = AXIS2_PLACEMENT_3D ( 'NONE', #3989, #12773, #11329 ) ;
#641 = CARTESIAN_POINT ( 'NONE',  ( -71.65000000218496723, 12.50000000000000000, 16.03553390593273420 ) ) ;
#642 = CARTESIAN_POINT ( 'NONE',  ( 2.445694354108820079, 2.445694354108820523, -1.387499998634402987 ) ) ;
#643 = CARTESIAN_POINT ( 'NONE',  ( 1.506022603841227436, 0.000000000000000000, 0.000000000000000000 ) ) ;
#644 = CARTESIAN_POINT ( 'NONE',  ( -3.458734124999998105, -1.432654583217642497, 18.75000000136560985 ) ) ;
#645 = CARTESIAN_POINT ( 'NONE',  ( 4.000000000000000888, 4.898587196589412829E-16, 11.50000000000001066 ) ) ;
#646 = CARTESIAN_POINT ( 'NONE',  ( 70.45000000109247651, 9.999999999999998224, 17.06698730000000097 ) ) ;
#647 = VECTOR ( 'NONE', #5180, 999.9999999999997726 ) ;
#648 = CARTESIAN_POINT ( 'NONE',  ( -1.655952806101422814, 3.662737355149034979, -7.623296525288699970E-18 ) ) ;
#649 = CARTESIAN_POINT ( 'NONE',  ( 53.93981816583844591, 10.06805114094563791, 17.99999999999999645 ) ) ;
#650 = CARTESIAN_POINT ( 'NONE',  ( -2.117863837641485618E-16, 3.458734125000000770, 5.737500001365596347 ) ) ;
#651 = CARTESIAN_POINT ( 'NONE',  ( -1.432654583217639166, 3.458734125000000770, 14.50000000136560629 ) ) ;
#652 = DIRECTION ( 'NONE',  ( -1.224646799147353207E-16, 0.000000000000000000, -1.000000000000000000 ) ) ;
#653 = CARTESIAN_POINT ( 'NONE',  ( -71.40000000109246514, 10.85617417291294551, 17.06698730000000097 ) ) ;
#654 = CARTESIAN_POINT ( 'NONE',  ( 7.010965453233809264, -9.000000000000003553, 5.000000000000079936 ) ) ;
#655 = ORIENTED_EDGE ( 'NONE', *, *, #23127, .T. ) ;
#656 = CARTESIAN_POINT ( 'NONE',  ( -2.712762565639006418, 3.052587955997511759, -3.430618716626627318 ) ) ;
#657 = CARTESIAN_POINT ( 'NONE',  ( 4.000000000000000000, 4.898587196589412829E-16, 4.925000002731187543 ) ) ;
#658 = CARTESIAN_POINT ( 'NONE',  ( -71.10000000109246798, 12.06698730000000275, 15.85617417291294196 ) ) ;
#659 = ORIENTED_EDGE ( 'NONE', *, *, #9537, .F. ) ;
#660 = VERTEX_POINT ( 'NONE', #8631 ) ;
#661 = CARTESIAN_POINT ( 'NONE',  ( 2.828427124746190735, -2.828427124746189847, 1.800000002731187987 ) ) ;
#662 = CARTESIAN_POINT ( 'NONE',  ( 4.000000000000000888, 4.898587196589412829E-16, 21.31370849898476649 ) ) ;
#663 = EDGE_LOOP ( 'NONE', ( #15328, #14805, #193, #15082 ) ) ;
#664 = CARTESIAN_POINT ( 'NONE',  ( 44.03180068014194148, -9.174246986850796759, 10.00000000000008704 ) ) ;
#665 = VECTOR ( 'NONE', #22333, 1000.000000000000000 ) ;
#666 = UNCERTAINTY_MEASURE_WITH_UNIT (LENGTH_MEASURE( 1.000000000000000082E-05 ), #20509, 'distance_accuracy_value', 'NONE');
#667 = CARTESIAN_POINT ( 'NONE',  ( 68.15000000109247935, 8.538419263543522320, 16.46158073645647235 ) ) ;
#668 = CARTESIAN_POINT ( 'NONE',  ( 69.50000000109247367, 10.85617417291294551, 12.93301269999999370 ) ) ;
#669 = VERTEX_POINT ( 'NONE', #23212 ) ;
#670 = AXIS2_PLACEMENT_3D ( 'NONE', #10554, #3674, #5368 ) ;
#671 = EDGE_CURVE ( 'NONE', #1632, #19016, #6131, .T. ) ;
#672 = CARTESIAN_POINT ( 'NONE',  ( 118.3095189484530181, 10.00000000000001599, 12.50000000000002309 ) ) ;
#673 =( BOUNDED_CURVE ( )  B_SPLINE_CURVE ( 2, ( #7283, #9203, #16490, #14354, #12440, #10774, #7037, #12692, #3655 ),
 .UNSPECIFIED., .F., .F. ) 
 B_SPLINE_CURVE_WITH_KNOTS ( ( 3, 2, 2, 2, 3 ),
 ( 0.05000000000000000278, 0.06250000000000000000, 0.07499999999999999722, 0.08749999999999999445, 0.1000000000000000056 ),
 .UNSPECIFIED. ) 
 CURVE ( )  GEOMETRIC_REPRESENTATION_ITEM ( )  RATIONAL_B_SPLINE_CURVE ( ( 1.000000000000000000, 0.9238795325112867385, 1.000000000000000000, 0.9238795325112867385, 1.000000000000000000, 0.9238795325112867385, 1.000000000000000000, 0.9238795325112867385, 1.000000000000000000 ) ) 
 REPRESENTATION_ITEM ( '' )  );
#674 = CARTESIAN_POINT ( 'NONE',  ( 57.09375000000000711, 11.65685424949236193, 10.99999999999998401 ) ) ;
#675 = PLANE ( 'NONE',  #14226 ) ;
#676 = CARTESIAN_POINT ( 'NONE',  ( -2.445694354108818303, -2.445694354108820523, 18.56250000136560629 ) ) ;
#677 = DIRECTION ( 'NONE',  ( 0.000000000000000000, 0.000000000000000000, -1.000000000000000000 ) ) ;
#678 = CIRCLE ( 'NONE', #6046, 4.000000000000001776 ) ;
#679 = VECTOR ( 'NONE', #7844, 999.9999999999998863 ) ;
#680 = DIRECTION ( 'NONE',  ( -1.000000000000000000, -0.000000000000000000, -0.000000000000000000 ) ) ;
#681 = ORIENTED_EDGE ( 'NONE', *, *, #21483, .T. ) ;
#682 = DIRECTION ( 'NONE',  ( 0.3420201433256622181, -0.9396926207859107594, 0.000000000000000000 ) ) ;
#683 = VERTEX_POINT ( 'NONE', #3814 ) ;
#684 = PRESENTATION_LAYER_ASSIGNMENT (  '', '', ( #18679 ) ) ;
#685 = CARTESIAN_POINT ( 'NONE',  ( 3.007318562400188799, 2.637429632093199139, 2.039999999999998259 ) ) ;
#686 = CARTESIAN_POINT ( 'NONE',  ( -70.54999999999999716, 11.03553390593272177, 12.49999999999998046 ) ) ;
#687 = ADVANCED_FACE ( 'NONE', ( #12941 ), #1773, .T. ) ;
#688 = ORIENTED_EDGE ( 'NONE', *, *, #7365, .T. ) ;
#689 = CARTESIAN_POINT ( 'NONE',  ( 118.3095189484530181, 10.00000000000001599, 34.11836509645782201 ) ) ;
#690 = LINE ( 'NONE', #6575, #22493 ) ;
#691 = CARTESIAN_POINT ( 'NONE',  ( -72.50000000000000000, 9.999999999999998224, 12.49999999999999289 ) ) ;
#692 = DIRECTION ( 'NONE',  ( 1.000000000000000000, 7.703719777548943412E-32, 0.000000000000000000 ) ) ;
#693 = ORIENTED_EDGE ( 'NONE', *, *, #18920, .T. ) ;
#694 = FACE_OUTER_BOUND ( 'NONE', #17938, .T. ) ;
#695 = ORIENTED_EDGE ( 'NONE', *, *, #8510, .F. ) ;
#696 = STYLED_ITEM ( 'NONE', ( #1788 ), #14725 ) ;
#697 = CYLINDRICAL_SURFACE ( 'NONE', #7614, 2.500000000000002220 ) ;
#698 = CARTESIAN_POINT ( 'NONE',  ( 4.000000000000000888, 1.656854249492381248, 16.56250000000001066 ) ) ;
#699 = CARTESIAN_POINT ( 'NONE',  ( 40.95362874676621345, -9.000000000000003553, 5.000000000000079936 ) ) ;
#700 = AXIS2_PLACEMENT_3D ( 'NONE', #22724, #17242, #13777 ) ;
#701 = VERTEX_POINT ( 'NONE', #9115 ) ;
#702 = DIRECTION ( 'NONE',  ( -0.000000000000000000, 0.000000000000000000, 1.000000000000000000 ) ) ;
#703 = CARTESIAN_POINT ( 'NONE',  ( -1.800000000000000711, 0.000000000000000000, 0.000000000000000000 ) ) ;
#704 = CARTESIAN_POINT ( 'NONE',  ( 71.50000000109247367, 9.143825827087049163, 17.06698730000000097 ) ) ;
#705 = ORIENTED_EDGE ( 'NONE', *, *, #16420, .F. ) ;
#706 = ADVANCED_FACE ( 'NONE', ( #20086 ), #19862, .T. ) ;
#707 = DIRECTION ( 'NONE',  ( -1.000000000000000000, 0.000000000000000000, 0.000000000000000000 ) ) ;
#708 = ADVANCED_FACE ( 'NONE', ( #10683 ), #16403, .F. ) ;
#709 = DIRECTION ( 'NONE',  ( -0.000000000000000000, -0.000000000000000000, -1.000000000000000000 ) ) ;
#710 = CIRCLE ( 'NONE', #20208, 8.749000000000002331 ) ;
#711 = CARTESIAN_POINT ( 'NONE',  ( 70.70000000109247651, 9.143825827087049163, 17.06698729999999742 ) ) ;
#712 = CARTESIAN_POINT ( 'NONE',  ( 2.445694354108821855, -2.445694354108820079, 11.81250000136560629 ) ) ;
#713 = DIRECTION ( 'NONE',  ( -0.000000000000000000, -0.000000000000000000, 1.000000000000000000 ) ) ;
#714 = VECTOR ( 'NONE', #9364, 1000.000000000000000 ) ;
#715 = CARTESIAN_POINT ( 'NONE',  ( 6.500000000000002665, 1.277696550142691345, -0.05601745114479450560 ) ) ;
#716 = EDGE_LOOP ( 'NONE', ( #13134, #16758, #95, #16262 ) ) ;
#717 = CARTESIAN_POINT ( 'NONE',  ( -2.449293598294706907E-16, 4.000000000000000000, 1.050000000000000488 ) ) ;
#718 = CYLINDRICAL_SURFACE ( 'NONE', #10195, 6.735000000000022524 ) ;
#719 = LINE ( 'NONE', #4557, #8184 ) ;
#720 = CARTESIAN_POINT ( 'NONE',  ( 1.656854249492380138, 4.000000000000000000, -1.012499999999997291 ) ) ;
#721 = ADVANCED_FACE ( 'NONE', ( #14507 ), #11026, .T. ) ;
#722 = PRODUCT_DEFINITION_SHAPE ( 'NONE', 'NONE',  #23714 ) ;
#723 = EDGE_CURVE ( 'NONE', #9984, #9912, #18309, .T. ) ;
#724 = ORIENTED_EDGE ( 'NONE', *, *, #7005, .T. ) ;
#725 = CARTESIAN_POINT ( 'NONE',  ( -3.999999999999999112, 0.000000000000000000, 16.12500000273119838 ) ) ;
#726 = ORIENTED_EDGE ( 'NONE', *, *, #16884, .F. ) ;
#727 = CARTESIAN_POINT ( 'NONE',  ( 58.21875000000000711, 14.00000000000000888, 16.65685424949235482 ) ) ;
#728 = CARTESIAN_POINT ( 'NONE',  ( -67.80000000109247082, 9.143825827087050939, 12.93301269999999370 ) ) ;
#729 = ITEM_DEFINED_TRANSFORMATION ( 'NONE', 'NONE', #7633,  #7318 ) ;
#730 = AXIS2_PLACEMENT_3D ( 'NONE', #7144, #14338, #16358 ) ;
#731 = EDGE_LOOP ( 'NONE', ( #13217, #18222 ) ) ;
#732 = CARTESIAN_POINT ( 'NONE',  ( 0.000000000000000000, 0.000000000000000000, 0.000000000000000000 ) ) ;
#733 = EDGE_LOOP ( 'NONE', ( #2981, #9011 ) ) ;
#734 = AXIS2_PLACEMENT_3D ( 'NONE', #20200, #14854, #5488 ) ;
#735 = VERTEX_POINT ( 'NONE', #17959 ) ;
#736 = CARTESIAN_POINT ( 'NONE',  ( -2.445694354108818303, -2.445694354108820967, 16.81250000136560629 ) ) ;
#737 = AXIS2_PLACEMENT_3D ( 'NONE', #5154, #15229, #702 ) ;
#738 = CARTESIAN_POINT ( 'NONE',  ( 55.50000000000000711, 12.12132034355963484, 12.87867965644034740 ) ) ;
#739 = AXIS2_PLACEMENT_3D ( 'NONE', #1765, #7059, #9105 ) ;
#740 = CARTESIAN_POINT ( 'NONE',  ( -68.40000000109249356, 9.143825827087050939, 12.93301269999999370 ) ) ;
#741 = CARTESIAN_POINT ( 'NONE',  ( 70.60000000109246798, 7.933012699999995476, 15.85617417291294196 ) ) ;
#742 = CARTESIAN_POINT ( 'NONE',  ( -65.90000000109246514, 9.143825827087049163, 17.06698729999999742 ) ) ;
#743 = EDGE_CURVE ( 'NONE', #7467, #16789, #1892, .T. ) ;
#744 = CYLINDRICAL_SURFACE ( 'NONE', #19501, 4.999999999999996447 ) ;
#745 = CARTESIAN_POINT ( 'NONE',  ( 57.62268183416157541, 12.07320092032950676, 17.16943976678977180 ) ) ;
#746 = CARTESIAN_POINT ( 'NONE',  ( -19.99999999999999645, -9.000000000000003553, 5.000000000000079936 ) ) ;
#747 = CARTESIAN_POINT ( 'NONE',  ( 1.432654583217642275, -3.458734124999999882, 3.300000001365598568 ) ) ;
#748 = CARTESIAN_POINT ( 'NONE',  ( 72.50000000000000000, 9.999999999999998224, 17.49999999999999645 ) ) ;
#749 = CARTESIAN_POINT ( 'NONE',  ( -3.999999999999998224, -1.656854249492383246, 13.18750000273119660 ) ) ;
#750 = VECTOR ( 'NONE', #3701, 1000.000000000000114 ) ;
#751 = CARTESIAN_POINT ( 'NONE',  ( 72.05000000109247082, 9.999999999999998224, 17.06698730000000097 ) ) ;
#752 = ADVANCED_FACE ( 'NONE', ( #2001 ), #7785, .T. ) ;
#753 = EDGE_CURVE ( 'NONE', #22275, #18422, #5493, .T. ) ;
#754 = VECTOR ( 'NONE', #8335, 1000.000000000000000 ) ;
#755 = ORIENTED_EDGE ( 'NONE', *, *, #2170, .F. ) ;
#756 = CARTESIAN_POINT ( 'NONE',  ( -2.828427124746189403, 2.828427124746190291, 17.00000000273119838 ) ) ;
#757 = ORIENTED_EDGE ( 'NONE', *, *, #9423, .F. ) ;
#758 = CARTESIAN_POINT ( 'NONE',  ( 59.77893183416158962, 8.825410453826341595, 11.97181229448535511 ) ) ;
#759 =( NAMED_UNIT ( * ) SI_UNIT ( $, .STERADIAN. ) SOLID_ANGLE_UNIT ( ) );
#760 = CARTESIAN_POINT ( 'NONE',  ( 1.432654583217639832, 3.458734125000000326, 1.425000001365596791 ) ) ;
#761 = CARTESIAN_POINT ( 'NONE',  ( 2.445694354108820523, -2.445694354108820079, -0.8874999986344025427 ) ) ;
#762 = ORIENTED_EDGE ( 'NONE', *, *, #13154, .F. ) ;
#763 = VECTOR ( 'NONE', #682, 1000.000000000000114 ) ;
#764 = CARTESIAN_POINT ( 'NONE',  ( 1.656854249492384135, -3.999999999999999112, 14.31250000000001066 ) ) ;
#765 = VECTOR ( 'NONE', #19219, 1000.000000000000114 ) ;
#766 = LINE ( 'NONE', #2680, #12959 ) ;
#767 = ORIENTED_EDGE ( 'NONE', *, *, #14910, .F. ) ;
#768 = CARTESIAN_POINT ( 'NONE',  ( -69.20000000218495018, 12.50000000000000000, 14.99999999999999645 ) ) ;
#769 = CARTESIAN_POINT ( 'NONE',  ( 1.432654583217642053, -3.458734124999999882, -1.699999998634403875 ) ) ;
#770 = VECTOR ( 'NONE', #3245, 1000.000000000000000 ) ;
#771 = DIRECTION ( 'NONE',  ( 1.000000000000000000, 0.000000000000000000, 1.040834085586083271E-15 ) ) ;
#772 = CARTESIAN_POINT ( 'NONE',  ( 2.445694354108822299, -2.445694354108820079, 18.06250000136560274 ) ) ;
#773 = CARTESIAN_POINT ( 'NONE',  ( -71.29999999999998295, 9.999999999999998224, 12.49999999999999289 ) ) ;
#774 = VECTOR ( 'NONE', #12841, 1000.000000000000000 ) ;
#775 = CARTESIAN_POINT ( 'NONE',  ( 70.40000000109250777, 10.85617417291294551, 17.06698729999999742 ) ) ;
#776 = CARTESIAN_POINT ( 'NONE',  ( 70.70000000218495018, 11.76776695296636888, 13.23223304703362579 ) ) ;
#777 = AXIS2_PLACEMENT_3D ( 'NONE', #21806, #19998, #1567 ) ;
#778 = CARTESIAN_POINT ( 'NONE',  ( 54.12731816583844591, 12.16943976678978601, 17.07320092032949432 ) ) ;
#779 = CARTESIAN_POINT ( 'NONE',  ( -1.432654583217640942, -3.458734124999999882, -3.074999998634404541 ) ) ;
#780 = CARTESIAN_POINT ( 'NONE',  ( 3.458734125000001658, 1.432654583217640498, 12.25000000136560452 ) ) ;
#781 = ADVANCED_FACE ( 'NONE', ( #23460 ), #8880, .F. ) ;
#782 = LINE ( 'NONE', #8468, #11502 ) ;
#783 = CARTESIAN_POINT ( 'NONE',  ( -68.40000000109246514, 7.933012699999995476, 15.85617417291294196 ) ) ;
#784 = EDGE_CURVE ( 'NONE', #20532, #22990, #16520, .T. ) ;
#785 = FACE_OUTER_BOUND ( 'NONE', #1269, .T. ) ;
#786 = LINE ( 'NONE', #11832, #6692 ) ;
#787 = ORIENTED_EDGE ( 'NONE', *, *, #23119, .F. ) ;
#788 = LINE ( 'NONE', #2452, #19506 ) ;
#789 = CARTESIAN_POINT ( 'NONE',  ( -2.828427124746190291, 2.828427124746190291, 5.300000002731187543 ) ) ;
#790 = CARTESIAN_POINT ( 'NONE',  ( -69.45000000109247651, 12.06698730000000097, 14.99999999999999645 ) ) ;
#791 = ORIENTED_EDGE ( 'NONE', *, *, #17900, .F. ) ;
#792 = ORIENTED_EDGE ( 'NONE', *, *, #18099, .T. ) ;
#793 = CARTESIAN_POINT ( 'NONE',  ( 72.50000000000000000, 9.999999999999998224, 12.49999999999999289 ) ) ;
#794 = DIRECTION ( 'NONE',  ( 1.000000000000000000, 0.000000000000000000, 0.000000000000000000 ) ) ;
#795 = EDGE_LOOP ( 'NONE', ( #3413, #2892, #4216, #3819, #4414, #8132, #9324, #7494, #20640, #8419, #9699, #7965, #332, #11494, #6870, #4116, #6329, #19356, #12885, #18929, #9383, #2214 ) ) ;
#796 = DIRECTION ( 'NONE',  ( -1.000000000000000000, -7.703719777548943412E-32, 0.000000000000000000 ) ) ;
#797 = VECTOR ( 'NONE', #16186, 1000.000000000000227 ) ;
#798 = CARTESIAN_POINT ( 'NONE',  ( 68.70000000109246230, 12.06698730000000275, 15.85617417291294196 ) ) ;
#799 = CARTESIAN_POINT ( 'NONE',  ( 68.70000000109246230, 10.85617417291294551, 12.93301269999999370 ) ) ;
#800 = ORIENTED_EDGE ( 'NONE', *, *, #8131, .T. ) ;
#801 = FACE_OUTER_BOUND ( 'NONE', #1222, .T. ) ;
#802 = CARTESIAN_POINT ( 'NONE',  ( 58.68750000000000000, 9.999999999999978684, 10.99999999999999645 ) ) ;
#803 = CARTESIAN_POINT ( 'NONE',  ( -1.432654583217638944, 3.458734125000000326, 18.25000000136560629 ) ) ;
#804 = CIRCLE ( 'NONE', #6927, 4.250000000000000000 ) ;
#805 = DIRECTION ( 'NONE',  ( 0.000000000000000000, 0.000000000000000000, 1.000000000000000000 ) ) ;
#806 = DIRECTION ( 'NONE',  ( 0.000000000000000000, 0.000000000000000000, 1.000000000000000000 ) ) ;
#807 = ORIENTED_EDGE ( 'NONE', *, *, #21186, .F. ) ;
#808 = CARTESIAN_POINT ( 'NONE',  ( 0.000000000000000000, 2.357898499370431722, -2.818925648462311528E-15 ) ) ;
#809 = CARTESIAN_POINT ( 'NONE',  ( -65.00000000000000000, 9.999999999999998224, 14.99999999999999645 ) ) ;
#810 = CARTESIAN_POINT ( 'NONE',  ( 4.999999999999999112, 0.000000000000000000, 0.000000000000000000 ) ) ;
#811 = ORIENTED_EDGE ( 'NONE', *, *, #17044, .F. ) ;
#812 = DIRECTION ( 'NONE',  ( -1.000000000000000000, 0.000000000000000000, 0.000000000000000000 ) ) ;
#813 = PLANE ( 'NONE',  #14115 ) ;
#814 = PLANE ( 'NONE',  #15172 ) ;
#815 = CARTESIAN_POINT ( 'NONE',  ( 71.20000000218495018, 7.499999999999996447, 14.99999999999999645 ) ) ;
#816 = ORIENTED_EDGE ( 'NONE', *, *, #15740, .F. ) ;
#817 = DIRECTION ( 'NONE',  ( -1.000000000000000000, -0.000000000000000000, 0.000000000000000000 ) ) ;
#818 = EDGE_LOOP ( 'NONE', ( #23139, #22622, #21693, #4272 ) ) ;
#819 = ADVANCED_FACE ( 'NONE', ( #14739 ), #5612, .T. ) ;
#820 = FACE_OUTER_BOUND ( 'NONE', #22082, .T. ) ;
#821 = CARTESIAN_POINT ( 'NONE',  ( 4.000000000000000888, 1.656854249492381248, 12.56250000000001243 ) ) ;
#822 = CARTESIAN_POINT ( 'NONE',  ( 71.45000000218495018, 11.03553390593273598, 12.49999999999999289 ) ) ;
#823 = CARTESIAN_POINT ( 'NONE',  ( 4.000000000000000888, 4.898587196589412829E-16, 19.50000000000001066 ) ) ;
#824 =( BOUNDED_CURVE ( )  B_SPLINE_CURVE ( 2, ( #13954, #15639, #17660, #1221, #6398, #22911, #21329, #10248, #6525 ),
 .UNSPECIFIED., .F., .F. ) 
 B_SPLINE_CURVE_WITH_KNOTS ( ( 3, 2, 2, 2, 3 ),
 ( 0.000000000000000000, 0.01250000000000000243, 0.02500000000000000486, 0.03749999999999999861, 0.05000000000000000971 ),
 .UNSPECIFIED. ) 
 CURVE ( )  GEOMETRIC_REPRESENTATION_ITEM ( )  RATIONAL_B_SPLINE_CURVE ( ( 1.000000000000000000, 0.9238795325112867385, 1.000000000000000000, 0.9238795325112867385, 1.000000000000000000, 0.9238795325112867385, 1.000000000000000000, 0.9238795325112867385, 1.000000000000000000 ) ) 
 REPRESENTATION_ITEM ( '' )  );
#825 = DIRECTION ( 'NONE',  ( 1.000000000000000000, 7.703719777548943412E-32, 0.000000000000000000 ) ) ;
#826 = CARTESIAN_POINT ( 'NONE',  ( 68.30000000109247082, 9.143825827087049163, 17.06698730000000097 ) ) ;
#827 = ORIENTED_EDGE ( 'NONE', *, *, #615, .T. ) ;
#828 = LINE ( 'NONE', #8044, #7240 ) ;
#829 = CARTESIAN_POINT ( 'NONE',  ( 70.65000000109246514, 9.999999999999998224, 17.06698730000000097 ) ) ;
#830 = CARTESIAN_POINT ( 'NONE',  ( 1.872352939448454495E-15, -3.458734125000000326, 11.68750000136560629 ) ) ;
#831 = DIRECTION ( 'NONE',  ( -1.000000000000000000, 0.000000000000000000, 1.239088197126290817E-16 ) ) ;
#832 = CYLINDRICAL_SURFACE ( 'NONE', #7334, 4.999999999999997335 ) ;
#833 = ORIENTED_EDGE ( 'NONE', *, *, #15388, .F. ) ;
#834 = CARTESIAN_POINT ( 'NONE',  ( -1.656854249492381248, -3.999999999999999112, 0.4875000000000020983 ) ) ;
#835 = CARTESIAN_POINT ( 'NONE',  ( 4.999999999999999112, -5.538577986808850717, -6.772677083992447500 ) ) ;
#836 = CARTESIAN_POINT ( 'NONE',  ( 1.872352939448454495E-15, -3.458734125000000326, 10.68750000136560452 ) ) ;
#837 = ORIENTED_EDGE ( 'NONE', *, *, #7035, .F. ) ;
#838 = CARTESIAN_POINT ( 'NONE',  ( -67.10000000109248219, 12.06698729999999919, 15.85617417291294196 ) ) ;
#839 = VERTEX_POINT ( 'NONE', #9344 ) ;
#840 = CARTESIAN_POINT ( 'NONE',  ( -68.10000000109245377, 12.06698730000000275, 15.85617417291294196 ) ) ;
#841 = CONTEXT_DEPENDENT_SHAPE_REPRESENTATION ( #16968, #17189 ) ;
#842 = EDGE_LOOP ( 'NONE', ( #23082, #13876, #7891, #7319, #20724, #21264 ) ) ;
#843 = DIRECTION ( 'NONE',  ( 0.000000000000000000, -0.3090169943749548342, 0.9510565162951509777 ) ) ;
#844 = VERTEX_POINT ( 'NONE', #16632 ) ;
#845 = EDGE_CURVE ( 'NONE', #11486, #18141, #210, .T. ) ;
#846 = EDGE_CURVE ( 'NONE', #18380, #19075, #883, .T. ) ;
#847 = EDGE_LOOP ( 'NONE', ( #5138, #11066, #23192, #10862, #4554, #15889, #19500, #15432, #12929, #23131 ) ) ;
#848 = CARTESIAN_POINT ( 'NONE',  ( -2.445694354108818303, -2.445694354108820967, 13.81250000136560629 ) ) ;
#849 = CARTESIAN_POINT ( 'NONE',  ( -68.60000000109248219, 12.06698730000000275, 14.14382582708705094 ) ) ;
#850 = CIRCLE ( 'NONE', #9294, 6.000000000000000888 ) ;
#851 = CARTESIAN_POINT ( 'NONE',  ( 70.15000000109247935, 11.46158073645647235, 13.53841926354352232 ) ) ;
#852 = ADVANCED_FACE ( 'NONE', ( #10150 ), #10485, .T. ) ;
#853 = CARTESIAN_POINT ( 'NONE',  ( -67.95000000109247651, 11.46158073645647235, 13.53841926354352232 ) ) ;
#854 = CARTESIAN_POINT ( 'NONE',  ( 6.500000000000000000, -0.6341575537611441327, 4.794206481459339919E-16 ) ) ;
#855 = CARTESIAN_POINT ( 'NONE',  ( 55.27893183416158251, 8.825410453826341595, 11.97181229448535511 ) ) ;
#856 = PLANE ( 'NONE',  #19991 ) ;
#857 = CARTESIAN_POINT ( 'NONE',  ( 3.458734125000000770, 1.432654583217640498, 3.550000001365598568 ) ) ;
#858 = LINE ( 'NONE', #4584, #16612 ) ;
#859 = CARTESIAN_POINT ( 'NONE',  ( -3.999999999999999112, 0.000000000000000000, 10.12500000273119660 ) ) ;
#860 = FACE_OUTER_BOUND ( 'NONE', #12699, .T. ) ;
#861 = EDGE_LOOP ( 'NONE', ( #16824, #10208, #1219, #4381 ) ) ;
#862 = CYLINDRICAL_SURFACE ( 'NONE', #15124, 4.000000000000001776 ) ;
#863 = EDGE_LOOP ( 'NONE', ( #11160, #1862, #19901, #14870 ) ) ;
#864 = CARTESIAN_POINT ( 'NONE',  ( 58.46643183416158251, 7.028187705514638672, 13.68930817193508531 ) ) ;
#865 = CARTESIAN_POINT ( 'NONE',  ( 3.458734125000000770, -1.432654583217639610, 0.1750000013655959585 ) ) ;
#866 = CARTESIAN_POINT ( 'NONE',  ( -3.458734125000000326, 1.432654583217640276, -0.3249999986344045411 ) ) ;
#867 = ORIENTED_EDGE ( 'NONE', *, *, #22089, .F. ) ;
#868 = DIRECTION ( 'NONE',  ( 1.000000000000000000, 7.703719777548943412E-32, 0.000000000000000000 ) ) ;
#869 = CARTESIAN_POINT ( 'NONE',  ( 50.00000000000000000, -14.69846310392956745, 35.82846581308617573 ) ) ;
#870 = CIRCLE ( 'NONE', #11634, 4.000000000000002665 ) ;
#871 = EDGE_CURVE ( 'NONE', #6822, #2402, #16754, .T. ) ;
#872 = VERTEX_POINT ( 'NONE', #13066 ) ;
#873 = DIRECTION ( 'NONE',  ( -0.000000000000000000, -1.000000000000000000, -0.000000000000000000 ) ) ;
#874 = ORIENTED_EDGE ( 'NONE', *, *, #14061, .F. ) ;
#875 = CARTESIAN_POINT ( 'NONE',  ( 57.03356816583845301, 11.31069182806492712, 17.97181229448534623 ) ) ;
#876 = CARTESIAN_POINT ( 'NONE',  ( -71.70000000218495018, 11.76776695296636888, 16.76776695296636532 ) ) ;
#877 = EDGE_CURVE ( 'NONE', #11647, #2759, #4374, .T. ) ;
#878 = DIRECTION ( 'NONE',  ( -0.000000000000000000, -0.000000000000000000, -1.000000000000000000 ) ) ;
#879 = ADVANCED_FACE ( 'NONE', ( #785 ), #15426, .F. ) ;
#880 = DIRECTION ( 'NONE',  ( 0.000000000000000000, 0.000000000000000000, 1.000000000000000000 ) ) ;
#881 = CARTESIAN_POINT ( 'NONE',  ( 66.59999999999999432, 11.76776695296636888, 13.23223304703362579 ) ) ;
#882 = CARTESIAN_POINT ( 'NONE',  ( 70.75000000109247367, 8.538419263543524096, 13.53841926354352054 ) ) ;
#883 = CIRCLE ( 'NONE', #20760, 6.760799999999997034 ) ;
#884 = CYLINDRICAL_SURFACE ( 'NONE', #4215, 4.000000000000001776 ) ;
#885 = CARTESIAN_POINT ( 'NONE',  ( 56.00231816583843170, 12.07320092032949610, 12.83056023321021044 ) ) ;
#886 = CARTESIAN_POINT ( 'NONE',  ( -1.432654583217641164, -3.458734125000000326, 5.175000001365595459 ) ) ;
#887 = CARTESIAN_POINT ( 'NONE',  ( 4.999999999999999112, 9.241976615262160522, -1.699438267350405818 ) ) ;
#888 = CARTESIAN_POINT ( 'NONE',  ( 67.35000000000000853, 11.03553390593276973, 12.50000000000002665 ) ) ;
#889 = CARTESIAN_POINT ( 'NONE',  ( -69.40000000109246514, 9.143825827087052716, 12.93301269999999192 ) ) ;
#890 = DIRECTION ( 'NONE',  ( 0.000000000000000000, 0.000000000000000000, 1.000000000000000000 ) ) ;
#891 = DIRECTION ( 'NONE',  ( -1.224646799147353207E-16, 0.000000000000000000, -1.000000000000000000 ) ) ;
#892 = VERTEX_POINT ( 'NONE', #11261 ) ;
#893 = CARTESIAN_POINT ( 'NONE',  ( -3.999999999999999112, 0.000000000000000000, 14.00000000000001066 ) ) ;
#894 =( NAMED_UNIT ( * ) PLANE_ANGLE_UNIT ( ) SI_UNIT ( $, .RADIAN. ) );
#895 = CARTESIAN_POINT ( 'NONE',  ( 2.828427124746189847, 2.828427124746190291, 5.050000002731187543 ) ) ;
#896 = ORIENTED_EDGE ( 'NONE', *, *, #11284, .F. ) ;
#897 = ORIENTED_EDGE ( 'NONE', *, *, #13576, .T. ) ;
#898 = CARTESIAN_POINT ( 'NONE',  ( 1.656854249492383024, -3.999999999999999112, 1.737500002731187543 ) ) ;
#899 = CLOSED_SHELL ( 'NONE', ( #6786, #11905, #3624, #2468, #18257, #22732, #4967, #5923, #20896, #22223, #13537, #1331, #3504, #3622, #20645, #21658, #19766, #6994, #8913, #3077, #23572, #6544, #2801, #1115, #10733, #19579, #15407, #6610, #17618, #7501, #9069, #8508, #2462, #21902, #20125, #19166, #8329, #3031, #5399, #13635, #21038, #15573, #18663, #22672 ) ) ;
#900 = DIRECTION ( 'NONE',  ( 1.000000000000000000, -0.000000000000000000, -1.224646799147353454E-16 ) ) ;
#901 = ORIENTED_EDGE ( 'NONE', *, *, #10609, .F. ) ;
#902 = CARTESIAN_POINT ( 'NONE',  ( 118.3095189484530181, -10.00000000000001954, 12.50000000000002132 ) ) ;
#903 = EDGE_CURVE ( 'NONE', #10781, #17912, #2563, .T. ) ;
#904 = EDGE_CURVE ( 'NONE', #21943, #17013, #4123, .T. ) ;
#905 = CARTESIAN_POINT ( 'NONE',  ( 67.75000000109247367, 11.46158073645647235, 13.53841926354352232 ) ) ;
#906 = EDGE_CURVE ( 'NONE', #14683, #16067, #1009, .T. ) ;
#907 = CARTESIAN_POINT ( 'NONE',  ( 68.45000000109247651, 7.933012699999995476, 14.99999999999999645 ) ) ;
#908 = PRODUCT ( 'socket head cap screw_iso_ISO 4762 M5 x 16 - 16N', 'socket head cap screw_iso_ISO 4762 M5 x 16 - 16N', '', ( #6130 ) ) ;
#909 = ORIENTED_EDGE ( 'NONE', *, *, #22823, .T. ) ;
#910 = CARTESIAN_POINT ( 'NONE',  ( 2.500000000000000000, 2.357898499370431722, -2.818925648462311528E-15 ) ) ;
#911 = CARTESIAN_POINT ( 'NONE',  ( 54.37500000000000711, 7.171572875253794166, 12.17157287525381726 ) ) ;
#912 = CYLINDRICAL_SURFACE ( 'NONE', #1944, 5.000000000000000888 ) ;
#913 = CARTESIAN_POINT ( 'NONE',  ( 1.872352939448454495E-15, -3.458734125000000326, 18.68750000136560629 ) ) ;
#914 = DIRECTION ( 'NONE',  ( -1.000000000000000000, -0.000000000000000000, -0.000000000000000000 ) ) ;
#915 = CARTESIAN_POINT ( 'NONE',  ( 16.42649855928345204, -8.974600000000002353, 5.000000000000079936 ) ) ;
#916 = ORIENTED_EDGE ( 'NONE', *, *, #11727, .T. ) ;
#917 = DIRECTION ( 'NONE',  ( -0.000000000000000000, -0.000000000000000000, -1.000000000000000000 ) ) ;
#918 = CARTESIAN_POINT ( 'NONE',  ( 50.00000000000000000, 15.00000000000003375, 34.11836509645780069 ) ) ;
#919 = CARTESIAN_POINT ( 'NONE',  ( 4.999999999999999112, 8.461683424509315543, 2.223716399045600145 ) ) ;
#920 = EDGE_LOOP ( 'NONE', ( #13456, #4533, #13927, #1880 ) ) ;
#921 = CARTESIAN_POINT ( 'NONE',  ( 69.30000000218494449, 11.76776695296636888, 16.76776695296636532 ) ) ;
#922 = CARTESIAN_POINT ( 'NONE',  ( 72.50000000000000000, 9.999999999999998224, 12.49999999999999289 ) ) ;
#923 = PRODUCT_DEFINITION_CONTEXT ( 'detailed design', #3030, 'design' ) ;
#924 = CIRCLE ( 'NONE', #14345, 4.000000000000001776 ) ;
#925 = CARTESIAN_POINT ( 'NONE',  ( 21.28513981966725765, -11.25000000000000355, 5.000000000000079936 ) ) ;
#926 = ORIENTED_EDGE ( 'NONE', *, *, #3827, .F. ) ;
#927 = CYLINDRICAL_SURFACE ( 'NONE', #10317, 4.000000000000000000 ) ;
#928 = ORIENTED_EDGE ( 'NONE', *, *, #4298, .F. ) ;
#929 = CARTESIAN_POINT ( 'NONE',  ( 71.85000000109246798, 12.06698730000000097, 14.99999999999999645 ) ) ;
#930 = VECTOR ( 'NONE', #15661, 1000.000000000000000 ) ;
#931 = AXIS2_PLACEMENT_3D ( 'NONE', #13447, #6358, #11652 ) ;
#932 = CARTESIAN_POINT ( 'NONE',  ( 70.70000000218495018, 11.76776695296636888, 13.23223304703362579 ) ) ;
#933 = CARTESIAN_POINT ( 'NONE',  ( -4.350525068611871049, 4.993776679985853839, -0.05533025579362114976 ) ) ;
#934 = CARTESIAN_POINT ( 'NONE',  ( 19.57733605323380743, -9.000000000000001776, 10.00000000000008882 ) ) ;
#935 = CARTESIAN_POINT ( 'NONE',  ( 68.10000000109246798, 12.06698729999999919, 15.85617417291294196 ) ) ;
#936 = ORIENTED_EDGE ( 'NONE', *, *, #12706, .F. ) ;
#937 = DIRECTION ( 'NONE',  ( 1.000000000000000000, 0.000000000000000000, 0.000000000000000000 ) ) ;
#938 = CARTESIAN_POINT ( 'NONE',  ( -19.55556463033274284, -11.25000000000000355, 10.00000000000008882 ) ) ;
#939 = CARTESIAN_POINT ( 'NONE',  ( 70.30000000109248504, 10.85617417291294551, 12.93301269999999370 ) ) ;
#940 = CARTESIAN_POINT ( 'NONE',  ( -3.458734124999998993, 1.432654583217640276, 14.37500000136560452 ) ) ;
#941 = VECTOR ( 'NONE', #12912, 1000.000000000000000 ) ;
#942 = CARTESIAN_POINT ( 'NONE',  ( 54.99999999999994316, -8.499999999999944933, 1.836970198721036294E-15 ) ) ;
#943 = EDGE_CURVE ( 'NONE', #15944, #21012, #11831, .T. ) ;
#944 = VECTOR ( 'NONE', #20944, 1000.000000000000114 ) ;
#945 = LINE ( 'NONE', #1062, #11167 ) ;
#946 = VERTEX_POINT ( 'NONE', #13176 ) ;
#947 = DIRECTION ( 'NONE',  ( 0.000000000000000000, 0.000000000000000000, 1.000000000000000000 ) ) ;
#948 = LINE ( 'NONE', #12006, #2112 ) ;
#949 = AXIS2_PLACEMENT_3D ( 'NONE', #6921, #17468, #12328 ) ;
#950 = CARTESIAN_POINT ( 'NONE',  ( 1.025207404391860050E-15, 3.458734125000000326, 10.18750000136560629 ) ) ;
#951 = CARTESIAN_POINT ( 'NONE',  ( -19.99999999999999645, -9.000000000000003553, 10.00000000000008882 ) ) ;
#952 = ORIENTED_EDGE ( 'NONE', *, *, #2709, .F. ) ;
#953 = DIRECTION ( 'NONE',  ( 0.000000000000000000, 0.000000000000000000, 1.000000000000000000 ) ) ;
#954 = EDGE_LOOP ( 'NONE', ( #23586, #9037, #13919, #18797 ) ) ;
#955 = CARTESIAN_POINT ( 'NONE',  ( -69.20000000109246230, 7.933012699999995476, 15.85617417291294196 ) ) ;
#956 = ORIENTED_EDGE ( 'NONE', *, *, #4066, .T. ) ;
#957 = CARTESIAN_POINT ( 'NONE',  ( 4.999999999999999112, 7.958834565716877307, -7.593217523260494595 ) ) ;
#958 = EDGE_LOOP ( 'NONE', ( #20659, #18197, #9065, #7020 ) ) ;
#959 =( BOUNDED_CURVE ( )  B_SPLINE_CURVE ( 2, ( #685, #9940, #4405 ),
 .UNSPECIFIED., .F., .F. ) 
 B_SPLINE_CURVE_WITH_KNOTS ( ( 3, 3 ),
 ( 0.3385621442156623861, 0.3499999999999999778 ),
 .UNSPECIFIED. ) 
 CURVE ( )  GEOMETRIC_REPRESENTATION_ITEM ( )  RATIONAL_B_SPLINE_CURVE ( ( 0.9881630579574953721, 0.9303476056502189007, 1.000000000000000000 ) ) 
 REPRESENTATION_ITEM ( '' )  );
#960 = ORIENTED_EDGE ( 'NONE', *, *, #723, .F. ) ;
#961 = CARTESIAN_POINT ( 'NONE',  ( 3.458734125000001658, 4.235727675282972223E-16, 13.18750000136560452 ) ) ;
#962 = CARTESIAN_POINT ( 'NONE',  ( 51.75000000000000711, 7.878679656440361612, 17.12132034355964549 ) ) ;
#963 = VECTOR ( 'NONE', #16673, 1000.000000000000114 ) ;
#964 = DIRECTION ( 'NONE',  ( 0.3420201433256622181, 0.9396926207859107594, -6.162975822039141593E-32 ) ) ;
#965 = VECTOR ( 'NONE', #15334, 1000.000000000000000 ) ;
#966 = LINE ( 'NONE', #19402, #21718 ) ;
#967 = CARTESIAN_POINT ( 'NONE',  ( -70.95000000000000284, 8.964466094067258695, 17.50000000000000355 ) ) ;
#968 = CARTESIAN_POINT ( 'NONE',  ( 45.00000000000000000, -10.00000000000001954, 15.00000000000002842 ) ) ;
#969 = CARTESIAN_POINT ( 'NONE',  ( 60.62268183416157541, 12.78030770151606177, 17.87654654797631792 ) ) ;
#970 = CARTESIAN_POINT ( 'NONE',  ( 0.000000000000000000, 6.807171995660585395, 6.478011392632914145 ) ) ;
#971 = AXIS2_PLACEMENT_3D ( 'NONE', #12093, #6451, #13770 ) ;
#972 = EDGE_CURVE ( 'NONE', #299, #5121, #23059, .T. ) ;
#973 = CARTESIAN_POINT ( 'NONE',  ( 3.458734125000001214, -1.432654583217639610, 3.425000001365596791 ) ) ;
#974 = EDGE_CURVE ( 'NONE', #20062, #17653, #8116, .T. ) ;
#975 = LINE ( 'NONE', #6510, #11280 ) ;
#976 = CARTESIAN_POINT ( 'NONE',  ( 1.656854249492384135, -3.999999999999999112, 13.43750000273119838 ) ) ;
#977 = DIRECTION ( 'NONE',  ( 0.3373062947069098150, -0.9413949561959078505, 0.000000000000000000 ) ) ;
#978 = B_SPLINE_CURVE_WITH_KNOTS ( 'NONE', 3,
 ( #7008, #16230, #8938, #21585, #12539, #19802 ),
 .UNSPECIFIED., .F., .F.,
 ( 4, 2, 4 ),
 ( 0.003358874760055550156, 0.004541967308452096383, 0.005725059856848641743 ),
 .UNSPECIFIED. ) ;
#979 = ORIENTED_EDGE ( 'NONE', *, *, #3064, .F. ) ;
#980 = CARTESIAN_POINT ( 'NONE',  ( -71.40000000218495302, 9.999999999999998224, 12.49999999999999289 ) ) ;
#981 = ORIENTED_EDGE ( 'NONE', *, *, #2562, .T. ) ;
#982 = CARTESIAN_POINT ( 'NONE',  ( 58.65393183416157541, 5.971812294485358663, 16.58880310854675599 ) ) ;
#983 = VECTOR ( 'NONE', #15941, 1000.000000000000000 ) ;
#984 = CARTESIAN_POINT ( 'NONE',  ( -2.445694354108820523, 2.445694354108820523, 0.6125000013655953479 ) ) ;
#985 = EDGE_CURVE ( 'NONE', #683, #21124, #19386, .T. ) ;
#986 = CARTESIAN_POINT ( 'NONE',  ( 3.458734125000000326, 1.432654583217640498, 1.300000001365597013 ) ) ;
#987 = ORIENTED_EDGE ( 'NONE', *, *, #1335, .T. ) ;
#988 = DIRECTION ( 'NONE',  ( 1.000000000000000000, 0.000000000000000000, 0.000000000000000000 ) ) ;
#989 = SURFACE_STYLE_FILL_AREA ( #6166 ) ;
#990 = VERTEX_POINT ( 'NONE', #7666 ) ;
#991 = DIRECTION ( 'NONE',  ( 1.000000000000000000, 0.000000000000000000, 0.000000000000000000 ) ) ;
#992 = ORIENTED_EDGE ( 'NONE', *, *, #12431, .F. ) ;
#993 = CARTESIAN_POINT ( 'NONE',  ( 50.28356816583843880, 8.275094609561968184, 11.02818770551464667 ) ) ;
#994 = CARTESIAN_POINT ( 'NONE',  ( -67.35000000218495586, 8.964466094067258695, 12.49999999999999289 ) ) ;
#995 = CARTESIAN_POINT ( 'NONE',  ( 2.500000000000000000, -2.357898499370432166, 3.035766082959412415E-15 ) ) ;
#996 = DIRECTION ( 'NONE',  ( -0.000000000000000000, -0.000000000000000000, -1.000000000000000000 ) ) ;
#997 = CARTESIAN_POINT ( 'NONE',  ( 66.40000000000000568, 8.232233047033629347, 13.23223304703362402 ) ) ;
#998 = CARTESIAN_POINT ( 'NONE',  ( 2.828427124746191179, 2.828427124746190291, 15.75000000273119660 ) ) ;
#999 = CARTESIAN_POINT ( 'NONE',  ( 1.600000000000004086, 0.000000000000000000, 0.000000000000000000 ) ) ;
#1000 = CARTESIAN_POINT ( 'NONE',  ( 71.20000000109246230, 10.85617417291294551, 17.06698729999999742 ) ) ;
#1001 = EDGE_CURVE ( 'NONE', #4177, #4376, #17325, .T. ) ;
#1002 = CARTESIAN_POINT ( 'NONE',  ( 4.999999999999999112, -10.90201369670499787, 1.464956435139505020 ) ) ;
#1003 = CARTESIAN_POINT ( 'NONE',  ( 54.40856816583843880, 12.97181229448534978, 13.68930817193506755 ) ) ;
#1004 = EDGE_CURVE ( 'NONE', #5469, #15347, #8225, .T. ) ;
#1005 = CARTESIAN_POINT ( 'NONE',  ( -1.432654583217641164, -3.458734125000000326, 3.175000001365598568 ) ) ;
#1006 = CARTESIAN_POINT ( 'NONE',  ( 1.432654583217643163, -3.458734124999999882, 13.00000000136560629 ) ) ;
#1007 = DIRECTION ( 'NONE',  ( 0.000000000000000000, 0.000000000000000000, 1.000000000000000000 ) ) ;
#1008 = CARTESIAN_POINT ( 'NONE',  ( -67.55000000109247082, 8.538419263543522320, 16.46158073645647235 ) ) ;
#1009 = LINE ( 'NONE', #6420, #5098 ) ;
#1010 = PLANE ( 'NONE',  #8594 ) ;
#1011 = EDGE_LOOP ( 'NONE', ( #3658, #10518, #13282, #21819 ) ) ;
#1012 = CARTESIAN_POINT ( 'NONE',  ( 4.000000000000000888, 4.898587196589412829E-16, 15.62500000273119660 ) ) ;
#1013 = PRESENTATION_STYLE_ASSIGNMENT (( #17448 ) ) ;
#1014 = LINE ( 'NONE', #20885, #4918 ) ;
#1015 = EDGE_CURVE ( 'NONE', #11403, #4148, #8182, .T. ) ;
#1016 = VERTEX_POINT ( 'NONE', #2809 ) ;
#1017 = EDGE_CURVE ( 'NONE', #3902, #22278, #8341, .T. ) ;
#1018 = ORIENTED_EDGE ( 'NONE', *, *, #12945, .T. ) ;
#1019 = LINE ( 'NONE', #13868, #23622 ) ;
#1020 = CARTESIAN_POINT ( 'NONE',  ( 0.000000000000000000, -9.314797388894900720, 1.239665997526853580 ) ) ;
#1021 = ORIENTED_EDGE ( 'NONE', *, *, #3597, .F. ) ;
#1022 = CARTESIAN_POINT ( 'NONE',  ( -0.1756481739660520902, 4.720212674038980261, -3.469390959564065291 ) ) ;
#1023 = CARTESIAN_POINT ( 'NONE',  ( 68.30000000109247082, 7.933012699999995476, 14.14382582708705094 ) ) ;
#1024 = AXIS2_PLACEMENT_3D ( 'NONE', #1199, #17638, #17514 ) ;
#1025 = CARTESIAN_POINT ( 'NONE',  ( 68.15000000109246514, 11.46158073645647235, 16.46158073645647235 ) ) ;
#1026 = EDGE_LOOP ( 'NONE', ( #16701, #10272, #6399, #3498 ) ) ;
#1027 = PLANE ( 'NONE',  #22161 ) ;
#1028 = CARTESIAN_POINT ( 'NONE',  ( 58.78125000000000711, 8.343145750507600766, 11.00000000000000533 ) ) ;
#1029 = EDGE_CURVE ( 'NONE', #4019, #13418, #23047, .T. ) ;
#1030 = CARTESIAN_POINT ( 'NONE',  ( 1.432654583217642275, -3.458734124999999437, 4.050000001365596347 ) ) ;
#1031 = CARTESIAN_POINT ( 'NONE',  ( -2.445694354108819191, 2.445694354108820523, 19.31250000136560629 ) ) ;
#1032 = DIRECTION ( 'NONE',  ( 0.000000000000000000, 0.3090169943749481174, -0.9510565162951533091 ) ) ;
#1033 = CONICAL_SURFACE ( 'NONE', #4476, 4.000000000000000000, 0.8911886515913786111 ) ;
#1034 = DIRECTION ( 'NONE',  ( -1.000000000000000000, 0.000000000000000000, 0.000000000000000000 ) ) ;
#1035 = VERTEX_POINT ( 'NONE', #21709 ) ;
#1036 = DIRECTION ( 'NONE',  ( 0.000000000000000000, 0.000000000000000000, -1.000000000000000000 ) ) ;
#1037 = EDGE_CURVE ( 'NONE', #23404, #17536, #10992, .T. ) ;
#1038 = FACE_OUTER_BOUND ( 'NONE', #18547, .T. ) ;
#1039 = CARTESIAN_POINT ( 'NONE',  ( 0.000000000000000000, 9.680994141368849171, -5.222868219166749704 ) ) ;
#1040 = AXIS2_PLACEMENT_3D ( 'NONE', #6929, #16381, #14603 ) ;
#1041 = AXIS2_PLACEMENT_3D ( 'NONE', #5177, #8916, #12519 ) ;
#1042 = EDGE_CURVE ( 'NONE', #11624, #2890, #19451, .T. ) ;
#1043 = ORIENTED_EDGE ( 'NONE', *, *, #13376, .T. ) ;
#1044 = DIRECTION ( 'NONE',  ( 1.000000000000000000, -0.000000000000000000, 0.000000000000000000 ) ) ;
#1045 = CARTESIAN_POINT ( 'NONE',  ( -6.170261003233799890, -9.000000000000005329, 10.00000000000008882 ) ) ;
#1046 = ORIENTED_EDGE ( 'NONE', *, *, #21323, .F. ) ;
#1047 = CARTESIAN_POINT ( 'NONE',  ( 71.70000000000000284, 9.999999999999998224, 17.49999999999999645 ) ) ;
#1048 = ORIENTED_EDGE ( 'NONE', *, *, #12159, .F. ) ;
#1049 = CARTESIAN_POINT ( 'NONE',  ( 2.828427124746191179, 2.828427124746190291, 17.62500000000001066 ) ) ;
#1050 = CARTESIAN_POINT ( 'NONE',  ( 69.75000000218496155, 8.964466094067258695, 12.49999999999999289 ) ) ;
#1051 = VECTOR ( 'NONE', #22738, 1000.000000000000000 ) ;
#1052 = PLANE ( 'NONE',  #16049 ) ;
#1053 = CARTESIAN_POINT ( 'NONE',  ( -3.999999999999999112, 0.000000000000000000, 12.00000000000001066 ) ) ;
#1054 = CARTESIAN_POINT ( 'NONE',  ( 68.40000000109246514, 7.933012699999995476, 15.85617417291294196 ) ) ;
#1055 = EDGE_LOOP ( 'NONE', ( #23220, #8381, #22152 ) ) ;
#1056 = CIRCLE ( 'NONE', #16771, 11.00000000000000000 ) ;
#1057 = LINE ( 'NONE', #8392, #23303 ) ;
#1058 = CARTESIAN_POINT ( 'NONE',  ( 65.00000000000000000, 9.999999999999998224, 19.99999999999999645 ) ) ;
#1059 = CARTESIAN_POINT ( 'NONE',  ( 69.60000000109248219, 12.06698730000000275, 14.14382582708705094 ) ) ;
#1060 = CARTESIAN_POINT ( 'NONE',  ( -1.432654583217639166, 3.458734125000000770, 18.50000000136560629 ) ) ;
#1061 = LINE ( 'NONE', #942, #17401 ) ;
#1062 = CARTESIAN_POINT ( 'NONE',  ( 72.50000000000000000, 9.999999999999998224, 12.49999999999999289 ) ) ;
#1063 = VERTEX_POINT ( 'NONE', #1358 ) ;
#1064 = CARTESIAN_POINT ( 'NONE',  ( 2.828427124746189847, 2.828427124746190291, -1.074999999999997735 ) ) ;
#1065 = CARTESIAN_POINT ( 'NONE',  ( 1.656854249492381470, 4.000000000000000000, 15.68750000000001066 ) ) ;
#1066 = DIRECTION ( 'NONE',  ( -1.000000000000000000, -0.000000000000000000, 0.000000000000000000 ) ) ;
#1067 = CARTESIAN_POINT ( 'NONE',  ( 54.99999999999992895, 15.00000000000000000, 1.836970198721037478E-15 ) ) ;
#1068 = ADVANCED_FACE ( 'NONE', ( #5321 ), #12664, .F. ) ;
#1069 = ORIENTED_EDGE ( 'NONE', *, *, #20166, .F. ) ;
#1070 = AXIS2_PLACEMENT_3D ( 'NONE', #18321, #15001, #13305 ) ;
#1071 = CARTESIAN_POINT ( 'NONE',  ( 6.499999999999999112, -3.752776749732574135, -0.5805565836007695601 ) ) ;
#1072 = ORIENTED_EDGE ( 'NONE', *, *, #8691, .F. ) ;
#1073 = CARTESIAN_POINT ( 'NONE',  ( -68.00000000109245946, 12.06698730000000275, 14.14382582708705094 ) ) ;
#1074 = CONTEXT_DEPENDENT_SHAPE_REPRESENTATION ( #7643, #2235 ) ;
#1075 = ORIENTED_EDGE ( 'NONE', *, *, #7209, .F. ) ;
#1076 = DIRECTION ( 'NONE',  ( 1.000000000000000000, 0.000000000000000000, 0.000000000000000000 ) ) ;
#1077 = ORIENTED_EDGE ( 'NONE', *, *, #7147, .T. ) ;
#1078 = CIRCLE ( 'NONE', #21277, 0.03079999999999923077 ) ;
#1079 = ORIENTED_EDGE ( 'NONE', *, *, #15144, .F. ) ;
#1080 = CARTESIAN_POINT ( 'NONE',  ( -3.458734124999999437, 1.432654583217640498, 11.62500000136560452 ) ) ;
#1081 = LINE ( 'NONE', #13691, #1932 ) ;
#1082 = CARTESIAN_POINT ( 'NONE',  ( -4.211140560182196957, 2.431303136016537803, -3.745885042887433514 ) ) ;
#1083 = CARTESIAN_POINT ( 'NONE',  ( 66.30000000109247082, 12.06698729999999919, 15.85617417291294196 ) ) ;
#1084 = CARTESIAN_POINT ( 'NONE',  ( -70.09999999999999432, 9.999999999999998224, 17.49999999999999645 ) ) ;
#1085 = LINE ( 'NONE', #4580, #2998 ) ;
#1086 = CARTESIAN_POINT ( 'NONE',  ( 58.46643183416158251, 6.028187705514633343, 13.27509460956200016 ) ) ;
#1087 = DIRECTION ( 'NONE',  ( -1.000000000000000000, 0.000000000000000000, 0.000000000000000000 ) ) ;
#1088 = VECTOR ( 'NONE', #20183, 1000.000000000000000 ) ;
#1089 = CARTESIAN_POINT ( 'NONE',  ( 2.445694354108820079, 2.445694354108820523, -1.387499998634402987 ) ) ;
#1090 = FACE_OUTER_BOUND ( 'NONE', #13284, .T. ) ;
#1091 = CARTESIAN_POINT ( 'NONE',  ( -10.00000000000000000, 0.000000000000000000, 0.000000000000000000 ) ) ;
#1092 = CARTESIAN_POINT ( 'NONE',  ( 4.000000000000000888, 4.898587196589412829E-16, 12.62500000273119660 ) ) ;
#1093 = CARTESIAN_POINT ( 'NONE',  ( 0.000000000000000000, 0.000000000000000000, 2.039999999999998259 ) ) ;
#1094 = ORIENTED_EDGE ( 'NONE', *, *, #6571, .T. ) ;
#1095 = CARTESIAN_POINT ( 'NONE',  ( -71.00000000109248788, 12.06698729999999919, 14.14382582708705094 ) ) ;
#1096 = ORIENTED_EDGE ( 'NONE', *, *, #6735, .F. ) ;
#1097 = CARTESIAN_POINT ( 'NONE',  ( 60.71643183416158962, 13.97181229448536399, 16.72490539043799629 ) ) ;
#1098 = FILL_AREA_STYLE ('',( #14054 ) ) ;
#1099 = VECTOR ( 'NONE', #15927, 1000.000000000000000 ) ;
#1100 = CARTESIAN_POINT ( 'NONE',  ( -2.445694354108819635, -2.445694354108820523, 0.8625000013655955700 ) ) ;
#1101 = ORIENTED_EDGE ( 'NONE', *, *, #21466, .F. ) ;
#1102 = CARTESIAN_POINT ( 'NONE',  ( -4.000000000000000000, 0.000000000000000000, 1.300000000000000711 ) ) ;
#1103 = AXIS2_PLACEMENT_3D ( 'NONE', #15008, #22627, #5874 ) ;
#1104 = ORIENTED_EDGE ( 'NONE', *, *, #9994, .F. ) ;
#1105 = DIRECTION ( 'NONE',  ( -1.000000000000000000, 0.000000000000000000, 0.000000000000000000 ) ) ;
#1106 = ORIENTED_EDGE ( 'NONE', *, *, #11011, .F. ) ;
#1107 = CARTESIAN_POINT ( 'NONE',  ( 57.59606816583843880, 11.17458954617364242, 11.97181229448534800 ) ) ;
#1108 = EDGE_CURVE ( 'NONE', #15525, #19779, #19565, .T. ) ;
#1109 = CARTESIAN_POINT ( 'NONE',  ( -66.35000000218495586, 7.499999999999995559, 16.03553390593273420 ) ) ;
#1110 = PLANE ( 'NONE',  #11015 ) ;
#1111 = DIRECTION ( 'NONE',  ( -0.9396926207859107594, -0.3420201433256623291, 1.540743955509804830E-32 ) ) ;
#1112 = CARTESIAN_POINT ( 'NONE',  ( -3.458734124999998105, -1.432654583217642497, 17.75000000136560274 ) ) ;
#1113 = CARTESIAN_POINT ( 'NONE',  ( -2.828427124746188515, -2.828427124746190735, 14.25000000273119660 ) ) ;
#1114 = VECTOR ( 'NONE', #23199, 1000.000000000000000 ) ;
#1115 = ADVANCED_FACE ( 'NONE', ( #10855 ), #15882, .T. ) ;
#1116 = DIRECTION ( 'NONE',  ( -1.000000000000000000, 0.000000000000000000, -0.000000000000000000 ) ) ;
#1117 = CARTESIAN_POINT ( 'NONE',  ( 68.50000000109247367, 10.85617417291294551, 12.93301269999999370 ) ) ;
#1118 = AXIS2_PLACEMENT_3D ( 'NONE', #1736, #20046, #10528 ) ;
#1119 = CARTESIAN_POINT ( 'NONE',  ( 70.80000000218494449, 12.50000000000000000, 14.99999999999999645 ) ) ;
#1120 = CARTESIAN_POINT ( 'NONE',  ( 50.93981816583844591, 10.06805114094563791, 17.99999999999999645 ) ) ;
#1121 = CARTESIAN_POINT ( 'NONE',  ( 6.353591512924457348E-16, -3.458734125000000770, 2.237500001365596791 ) ) ;
#1122 = DIRECTION ( 'NONE',  ( 1.000000000000000000, 7.703719777548943412E-32, 0.000000000000000000 ) ) ;
#1123 = CARTESIAN_POINT ( 'NONE',  ( -69.60000000109246798, 12.06698729999999919, 14.14382582708705094 ) ) ;
#1124 = ORIENTED_EDGE ( 'NONE', *, *, #15503, .T. ) ;
#1125 = CARTESIAN_POINT ( 'NONE',  ( -69.95000000218493597, 12.50000000000000000, 13.96446609406725692 ) ) ;
#1126 = VERTEX_POINT ( 'NONE', #6891 ) ;
#1127 = CARTESIAN_POINT ( 'NONE',  ( 1.971781867644420635E-15, -4.000000000000000000, 15.37500000273119660 ) ) ;
#1129 =( GEOMETRIC_REPRESENTATION_CONTEXT ( 3 ) GLOBAL_UNCERTAINTY_ASSIGNED_CONTEXT ( ( #15787 ) ) GLOBAL_UNIT_ASSIGNED_CONTEXT ( ( #16369, #16257, #18157 ) ) REPRESENTATION_CONTEXT ( 'NONE', 'WORKASPACE' ) );
#1128 =( NAMED_UNIT ( * ) PLANE_ANGLE_UNIT ( ) SI_UNIT ( $, .RADIAN. ) );
#1130 = CARTESIAN_POINT ( 'NONE',  ( -2.828427124746189403, -2.828427124746190735, -0.4499999972688122352 ) ) ;
#1131 = ORIENTED_EDGE ( 'NONE', *, *, #17544, .F. ) ;
#1132 = VERTEX_POINT ( 'NONE', #18132 ) ;
#1133 = CARTESIAN_POINT ( 'NONE',  ( -20.00000000000001066, 4.500000000000003553, -50.00000000000000000 ) ) ;
#1134 = DIRECTION ( 'NONE',  ( 0.000000000000000000, 0.000000000000000000, 1.000000000000000000 ) ) ;
#1135 = ORIENTED_EDGE ( 'NONE', *, *, #11327, .F. ) ;
#1136 = FACE_OUTER_BOUND ( 'NONE', #3145, .T. ) ;
#1137 = CIRCLE ( 'NONE', #23336, 9.000000000000021316 ) ;
#1138 = UNCERTAINTY_MEASURE_WITH_UNIT (LENGTH_MEASURE( 1.000000000000000082E-05 ), #18255, 'distance_accuracy_value', 'NONE');
#1139 = EDGE_CURVE ( 'NONE', #1949, #8348, #15996, .T. ) ;
#1140 = EDGE_CURVE ( 'NONE', #11837, #5919, #23282, .T. ) ;
#1141 = CARTESIAN_POINT ( 'NONE',  ( 66.75000000109247367, 8.538419263543524096, 13.53841926354352054 ) ) ;
#1142 = VECTOR ( 'NONE', #15800, 1000.000000000000000 ) ;
#1143 = AXIS2_PLACEMENT_3D ( 'NONE', #12271, #5410, #7224 ) ;
#1144 = CARTESIAN_POINT ( 'NONE',  ( 68.60000000109246798, 9.143825827087050939, 12.93301269999999370 ) ) ;
#1145 = EDGE_CURVE ( 'NONE', #17824, #12317, #15957, .T. ) ;
#1146 = DIRECTION ( 'NONE',  ( -1.000000000000000000, 0.000000000000000000, 0.000000000000000000 ) ) ;
#1147 = CARTESIAN_POINT ( 'NONE',  ( 0.000000000000000000, 0.000000000000000000, 0.000000000000000000 ) ) ;
#1148 = CARTESIAN_POINT ( 'NONE',  ( 55.68750000000000000, 9.999999999999978684, 10.99999999999999645 ) ) ;
#1149 = CARTESIAN_POINT ( 'NONE',  ( 2.445694354108820079, 2.445694354108820523, 5.362500001365596347 ) ) ;
#1150 = CARTESIAN_POINT ( 'NONE',  ( 2.445694354108821411, 2.445694354108820523, 16.06250000136560629 ) ) ;
#1151 = CARTESIAN_POINT ( 'NONE',  ( 45.00000000000000000, 10.00000000000001599, 34.11836509645781490 ) ) ;
#1152 = CARTESIAN_POINT ( 'NONE',  ( 0.000000000000000000, 0.000000000000000000, -4.000000000000000000 ) ) ;
#1153 = ORIENTED_EDGE ( 'NONE', *, *, #22526, .T. ) ;
#1154 = DIRECTION ( 'NONE',  ( 0.000000000000000000, 0.000000000000000000, -1.000000000000000000 ) ) ;
#1155 = DIRECTION ( 'NONE',  ( 0.3420201433256622736, 0.9396926207859106484, 0.000000000000000000 ) ) ;
#1156 = DIRECTION ( 'NONE',  ( 1.000000000000000000, -0.000000000000000000, -0.000000000000000000 ) ) ;
#1157 = VECTOR ( 'NONE', #6497, 1000.000000000000000 ) ;
#1158 = ORIENTED_EDGE ( 'NONE', *, *, #4205, .F. ) ;
#1159 = CARTESIAN_POINT ( 'NONE',  ( 60.00000000000000711, -15.00000000000000000, 19.99999999999999645 ) ) ;
#1160 = CARTESIAN_POINT ( 'NONE',  ( 71.50000000109248788, 7.933012699999995476, 14.14382582708705094 ) ) ;
#1161 = MECHANICAL_DESIGN_GEOMETRIC_PRESENTATION_REPRESENTATION (  '', ( #6537 ), #4181 ) ;
#1162 = EDGE_CURVE ( 'NONE', #12772, #14872, #1238, .T. ) ;
#1163 = DIRECTION ( 'NONE',  ( 1.000000000000000000, 0.000000000000000000, 0.000000000000000000 ) ) ;
#1164 = ORIENTED_EDGE ( 'NONE', *, *, #3803, .F. ) ;
#1165 = DIRECTION ( 'NONE',  ( -1.000000000000000000, 0.000000000000000000, 0.000000000000000000 ) ) ;
#1166 = ORIENTED_EDGE ( 'NONE', *, *, #12523, .F. ) ;
#1167 = CARTESIAN_POINT ( 'NONE',  ( -3.999999999999999112, 0.000000000000000000, 20.00000000000001066 ) ) ;
#1168 = EDGE_CURVE ( 'NONE', #10566, #15405, #10231, .T. ) ;
#1169 = CARTESIAN_POINT ( 'NONE',  ( 71.40000000218495302, 9.999999999999998224, 12.49999999999999289 ) ) ;
#1170 = CARTESIAN_POINT ( 'NONE',  ( -1.656854249492380138, -3.999999999999999112, 19.18750000000001066 ) ) ;
#1171 = CARTESIAN_POINT ( 'NONE',  ( -2.855764796983342624, 2.970025579236414082, -0.09382832055445475272 ) ) ;
#1172 = CARTESIAN_POINT ( 'NONE',  ( 67.65000000109247935, 7.933012699999995476, 14.99999999999999645 ) ) ;
#1173 = EDGE_CURVE ( 'NONE', #1978, #6221, #8576, .T. ) ;
#1174 = EDGE_LOOP ( 'NONE', ( #15577, #8700, #10430, #20512 ) ) ;
#1175 = VECTOR ( 'NONE', #13412, 1000.000000000000114 ) ;
#1176 = EDGE_CURVE ( 'NONE', #158, #17446, #12413, .T. ) ;
#1177 = APPLICATION_CONTEXT ( 'automotive_design' ) ;
#1178 = CARTESIAN_POINT ( 'NONE',  ( -15.00000000000001066, 10.00000000000000000, -49.99999999999999289 ) ) ;
#1179 = CARTESIAN_POINT ( 'NONE',  ( 4.999999999999999112, 0.000000000000000000, 0.000000000000000000 ) ) ;
#1180 = DIRECTION ( 'NONE',  ( 0.000000000000000000, 0.000000000000000000, 1.000000000000000000 ) ) ;
#1181 = CARTESIAN_POINT ( 'NONE',  ( 2.445694354108821855, -2.445694354108820079, 10.81250000136560452 ) ) ;
#1182 = DIRECTION ( 'NONE',  ( -1.000000000000000000, -0.000000000000000000, -0.000000000000000000 ) ) ;
#1183 = PLANE ( 'NONE',  #8483 ) ;
#1184 = ORIENTED_EDGE ( 'NONE', *, *, #8510, .T. ) ;
#1185 = CARTESIAN_POINT ( 'NONE',  ( 7.347880794884118750E-16, -4.000000000000000000, -1.449999999999998179 ) ) ;
#1186 = LINE ( 'NONE', #11771, #12491 ) ;
#1187 = DIRECTION ( 'NONE',  ( 0.000000000000000000, 0.000000000000000000, 1.000000000000000000 ) ) ;
#1188 = CARTESIAN_POINT ( 'NONE',  ( -72.15000000000001990, 11.03553390593275374, 12.50000000000001243 ) ) ;
#1189 = ORIENTED_EDGE ( 'NONE', *, *, #10837, .T. ) ;
#1190 = FACE_BOUND ( 'NONE', #7353, .T. ) ;
#1191 = ORIENTED_EDGE ( 'NONE', *, *, #21487, .F. ) ;
#1192 = CARTESIAN_POINT ( 'NONE',  ( 0.000000000000000000, 7.347880794884120722E-16, 6.000000000000000888 ) ) ;
#1193 = EDGE_LOOP ( 'NONE', ( #2380, #12041, #6105, #18841 ) ) ;
#1194 = DIRECTION ( 'NONE',  ( 0.000000000000000000, 0.000000000000000000, -1.000000000000000000 ) ) ;
#1195 = ORIENTED_EDGE ( 'NONE', *, *, #7139, .T. ) ;
#1196 = ORIENTED_EDGE ( 'NONE', *, *, #6597, .F. ) ;
#1197 = CARTESIAN_POINT ( 'NONE',  ( -1.432654583217639166, 3.458734125000000770, 13.50000000136560452 ) ) ;
#1198 = CARTESIAN_POINT ( 'NONE',  ( 51.37500000000000711, 7.878679656440349177, 12.87867965644035984 ) ) ;
#1199 = CARTESIAN_POINT ( 'NONE',  ( 4.999999999999999112, 0.000000000000000000, 0.000000000000000000 ) ) ;
#1200 = CARTESIAN_POINT ( 'NONE',  ( 65.65000000109247935, 9.999999999999998224, 17.06698730000000097 ) ) ;
#1201 = EDGE_CURVE ( 'NONE', #19518, #3871, #23160, .T. ) ;
#1202 = EDGE_CURVE ( 'NONE', #10547, #13807, #23402, .T. ) ;
#1203 = CARTESIAN_POINT ( 'NONE',  ( -69.05000000000002558, 12.50000000000000000, 13.96446609406725869 ) ) ;
#1204 = DIRECTION ( 'NONE',  ( -2.465190328815656418E-32, -0.3420201433256691015, 0.9396926207859083169 ) ) ;
#1205 = CARTESIAN_POINT ( 'NONE',  ( 60.00000000000001421, 11.22198354879773419, 18.10280442057481665 ) ) ;
#1206 = CARTESIAN_POINT ( 'NONE',  ( 3.458734125000001214, -1.432654583217639610, -0.5749999986344027647 ) ) ;
#1207 = CARTESIAN_POINT ( 'NONE',  ( -67.60000000218495586, 12.50000000000000000, 14.99999999999999645 ) ) ;
#1208 = CARTESIAN_POINT ( 'NONE',  ( 72.50000000000000000, 9.999999999999998224, 14.99999999999999645 ) ) ;
#1209 = CARTESIAN_POINT ( 'NONE',  ( -3.458734124999998993, -1.432654583217642497, 18.50000000136560629 ) ) ;
#1210 = LINE ( 'NONE', #8194, #8825 ) ;
#1211 = ORIENTED_EDGE ( 'NONE', *, *, #17544, .T. ) ;
#1212 = CARTESIAN_POINT ( 'NONE',  ( -71.95000000109247651, 11.46158073645647235, 16.46158073645647235 ) ) ;
#1213 = ORIENTED_EDGE ( 'NONE', *, *, #16976, .T. ) ;
#1214 = CARTESIAN_POINT ( 'NONE',  ( 59.68518183416157541, 10.06805114094561659, 10.99999999999999645 ) ) ;
#1215 = CARTESIAN_POINT ( 'NONE',  ( -70.25000000109247367, 12.06698730000000097, 14.99999999999999645 ) ) ;
#1216 = CARTESIAN_POINT ( 'NONE',  ( 27.56832511966726784, -11.25000000000000355, 5.000000000000079936 ) ) ;
#1217 = EDGE_LOOP ( 'NONE', ( #8451, #11418 ) ) ;
#1218 = DIRECTION ( 'NONE',  ( -1.000000000000000000, -7.703719777548943412E-32, 0.000000000000000000 ) ) ;
#1219 = ORIENTED_EDGE ( 'NONE', *, *, #17180, .F. ) ;
#1220 = AXIS2_PLACEMENT_3D ( 'NONE', #17110, #4292, #7783 ) ;
#1221 = CARTESIAN_POINT ( 'NONE',  ( -1.656854249492379472, 4.000000000000000000, 19.81250000000001776 ) ) ;
#1222 = EDGE_LOOP ( 'NONE', ( #3301, #17935, #17506, #2754 ) ) ;
#1223 = CARTESIAN_POINT ( 'NONE',  ( 55.06481816583844591, 6.999999999999998224, 15.06805114094563436 ) ) ;
#1224 = CARTESIAN_POINT ( 'NONE',  ( -65.80000000218494449, 9.999999999999998224, 12.49999999999999289 ) ) ;
#1225 = LINE ( 'NONE', #8456, #17873 ) ;
#1226 = LINE ( 'NONE', #8564, #6844 ) ;
#1227 = CARTESIAN_POINT ( 'NONE',  ( 3.458734125000001658, 1.432654583217640498, 14.25000000136560452 ) ) ;
#1228 = CARTESIAN_POINT ( 'NONE',  ( -1.656854249492379250, 4.000000000000000000, 14.93750000273119660 ) ) ;
#1229 = CARTESIAN_POINT ( 'NONE',  ( 59.34375000000000711, 8.757359312880723223, 18.00000000000000355 ) ) ;
#1230 = CARTESIAN_POINT ( 'NONE',  ( 2.499999999999999556, -4.762163868918205978, -9.915734732513268312 ) ) ;
#1231 = CARTESIAN_POINT ( 'NONE',  ( 57.28125000000000711, 8.757359312880703683, 11.99999999999999822 ) ) ;
#1232 = CARTESIAN_POINT ( 'NONE',  ( 3.458734125000001214, -1.432654583217639610, 2.425000001365597679 ) ) ;
#1233 = CARTESIAN_POINT ( 'NONE',  ( -3.458734124999999437, 1.432654583217640498, 11.62500000136560452 ) ) ;
#1234 =( NAMED_UNIT ( * ) SI_UNIT ( $, .STERADIAN. ) SOLID_ANGLE_UNIT ( ) );
#1235 = CARTESIAN_POINT ( 'NONE',  ( -67.60000000109246798, 7.933012699999995476, 15.85617417291294196 ) ) ;
#1236 = EDGE_CURVE ( 'NONE', #10607, #14136, #2968, .T. ) ;
#1237 = ORIENTED_EDGE ( 'NONE', *, *, #15576, .F. ) ;
#1238 = LINE ( 'NONE', #1710, #19369 ) ;
#1239 = CARTESIAN_POINT ( 'NONE',  ( -3.472371940586054251, -2.614027278893156669, -3.320322319202162031 ) ) ;
#1240 = EDGE_LOOP ( 'NONE', ( #9762, #18516, #602, #12286 ) ) ;
#1241 = CARTESIAN_POINT ( 'NONE',  ( 59.25000000000000711, 7.878679656440361612, 17.12132034355964549 ) ) ;
#1242 = SURFACE_STYLE_FILL_AREA ( #17329 ) ;
#1243 = CARTESIAN_POINT ( 'NONE',  ( -4.000000000000000000, 0.000000000000000000, 0.4250000027311868211 ) ) ;
#1244 = ORIENTED_EDGE ( 'NONE', *, *, #22795, .F. ) ;
#1245 = ORIENTED_EDGE ( 'NONE', *, *, #12789, .T. ) ;
#1246 = CARTESIAN_POINT ( 'NONE',  ( 1.876855952934447513, -6.421950209808290566, -0.1061556211655389631 ) ) ;
#1247 = DIRECTION ( 'NONE',  ( 0.000000000000000000, 0.000000000000000000, 1.000000000000000000 ) ) ;
#1248 = ORIENTED_EDGE ( 'NONE', *, *, #5366, .T. ) ;
#1249 = DIRECTION ( 'NONE',  ( 0.3420201433256622181, 0.9396926207859107594, -6.162975822039141593E-32 ) ) ;
#1250 = CARTESIAN_POINT ( 'NONE',  ( -69.50000000218494733, 8.232233047033627571, 16.76776695296636532 ) ) ;
#1251 = DIRECTION ( 'NONE',  ( -0.9396926207859107594, -0.3420201433256623291, 1.540743955509804830E-32 ) ) ;
#1252 = VECTOR ( 'NONE', #14860, 1000.000000000000000 ) ;
#1253 = CARTESIAN_POINT ( 'NONE',  ( 71.89999999999999147, 7.499999999999996447, 14.99999999999999645 ) ) ;
#1254 = VECTOR ( 'NONE', #21465, 1000.000000000000000 ) ;
#1255 = CYLINDRICAL_SURFACE ( 'NONE', #12424, 8.749000000000002331 ) ;
#1256 = DIRECTION ( 'NONE',  ( 1.224646799147353207E-16, -0.000000000000000000, 1.000000000000000000 ) ) ;
#1257 = CARTESIAN_POINT ( 'NONE',  ( 52.31250000000000711, 14.00000000000000000, 14.99999999999997691 ) ) ;
#1258 = CARTESIAN_POINT ( 'NONE',  ( -3.458734124999999882, -1.432654583217642497, 2.800000001365598123 ) ) ;
#1259 = CARTESIAN_POINT ( 'NONE',  ( -1.432654583217638944, 3.458734125000000326, 14.25000000136560452 ) ) ;
#1260 = PLANE ( 'NONE',  #10933 ) ;
#1261 = EDGE_CURVE ( 'NONE', #20390, #10320, #978, .T. ) ;
#1262 = CLOSED_SHELL ( 'NONE', ( #12173, #18259, #8900, #23265, #5232, #15888, #13041, #16982, #9204, #17816, #574, #17103, #7934, #5546, #10230, #18707, #15440, #22542, #13050, #17709, #6756, #18453, #617, #21807, #2163, #4498, #2772, #13616, #2395, #20898, #18963, #19011, #7497, #10766, #150, #14, #7174, #12851, #22115, #16736, #418, #2742, #8003, #7474, #4089, #21000, #19732, #13311, #23369, #1634, #6162, #12147, #583, #19221, #2764, #10870, #8072, #20362, #16524, #9978, #8833, #16699, #18694, #1640, #10577, #8731, #17549, #11935, #6437, #3995, #20006, #9569, #2734, #16844, #3919, #14186, #11659, #18299, #17450, #6002, #2025, #10895, #14620, #18769, #4674, #21395, #4890, #6632, #5534, #7372, #16124, #23427, #11393, #3371, #17557, #5197 ) ) ;
#1263 = DIRECTION ( 'NONE',  ( -1.000000000000000000, -0.000000000000000000, -0.000000000000000000 ) ) ;
#1264 = VERTEX_POINT ( 'NONE', #3404 ) ;
#1265 = CARTESIAN_POINT ( 'NONE',  ( -2.710465755160788248, 2.627675682436018789, 2.039999999999999591 ) ) ;
#1266 = EDGE_CURVE ( 'NONE', #1264, #22517, #13759, .T. ) ;
#1267 = CARTESIAN_POINT ( 'NONE',  ( 68.49999999999998579, 9.999999999999998224, 17.49999999999999645 ) ) ;
#1268 = LINE ( 'NONE', #10304, #1617 ) ;
#1269 = EDGE_LOOP ( 'NONE', ( #13649, #20440, #1072, #14194, #11128, #20415 ) ) ;
#1270 = CARTESIAN_POINT ( 'NONE',  ( 4.000000000000000888, 4.898587196589412829E-16, 13.62500000273119660 ) ) ;
#1271 = CYLINDRICAL_SURFACE ( 'NONE', #2645, 4.000000000000001776 ) ;
#1272 = EDGE_CURVE ( 'NONE', #22486, #7327, #22825, .T. ) ;
#1273 = CARTESIAN_POINT ( 'NONE',  ( 4.000000000000000000, 2.309401076758497151, -3.433295621305379353 ) ) ;
#1274 = EDGE_LOOP ( 'NONE', ( #12538, #14783, #7203, #5503 ) ) ;
#1275 = LINE ( 'NONE', #10311, #14119 ) ;
#1276 = ORIENTED_EDGE ( 'NONE', *, *, #7465, .F. ) ;
#1277 = CARTESIAN_POINT ( 'NONE',  ( 51.56250000000000711, 5.999999999999996447, 15.00000000000001599 ) ) ;
#1278 = CARTESIAN_POINT ( 'NONE',  ( 67.95000000218495018, 7.499999999999995559, 16.03553390593273420 ) ) ;
#1279 = CIRCLE ( 'NONE', #14335, 6.500000000000000888 ) ;
#1280 = DIRECTION ( 'NONE',  ( -1.224646799147353207E-16, 0.000000000000000000, -1.000000000000000000 ) ) ;
#1281 = DIRECTION ( 'NONE',  ( 1.224646799147353207E-16, -0.000000000000000000, 1.000000000000000000 ) ) ;
#1282 = CARTESIAN_POINT ( 'NONE',  ( 68.50000000109245946, 7.933012699999995476, 14.14382582708705094 ) ) ;
#1283 = EDGE_LOOP ( 'NONE', ( #5038, #4850, #609, #13055 ) ) ;
#1284 = CARTESIAN_POINT ( 'NONE',  ( 65.00000000000000000, -9.999999999999998224, 19.99999999999999645 ) ) ;
#1285 = ADVANCED_FACE ( 'NONE', ( #3744 ), #7930, .F. ) ;
#1286 = CARTESIAN_POINT ( 'NONE',  ( 2.499999999999999556, -5.222868219166923787, 9.680994141368751471 ) ) ;
#1287 = CARTESIAN_POINT ( 'NONE',  ( 67.05000000109247082, 9.999999999999998224, 12.93301269999999192 ) ) ;
#1288 = CARTESIAN_POINT ( 'NONE',  ( 3.458734125000001214, 4.235727675282971730E-16, 10.93750000136560452 ) ) ;
#1289 = CARTESIAN_POINT ( 'NONE',  ( -90.00000000000000000, 0.000000000000000000, -8.073750000000021743 ) ) ;
#1290 = EDGE_CURVE ( 'NONE', #129, #633, #2063, .T. ) ;
#1291 = DIRECTION ( 'NONE',  ( 1.000000000000000000, 0.000000000000000000, 0.000000000000000000 ) ) ;
#1292 = ORIENTED_EDGE ( 'NONE', *, *, #15053, .T. ) ;
#1293 = DIRECTION ( 'NONE',  ( -0.000000000000000000, -1.000000000000000000, 0.000000000000000000 ) ) ;
#1294 = EDGE_CURVE ( 'NONE', #4086, #4004, #9769, .T. ) ;
#1295 = CARTESIAN_POINT ( 'NONE',  ( 59.90625000000000711, 12.99999999999999645, 13.75735931288070191 ) ) ;
#1296 = CARTESIAN_POINT ( 'NONE',  ( 66.74999999999998579, 12.50000000000000000, 16.03553390593273775 ) ) ;
#1297 = VERTEX_POINT ( 'NONE', #7729 ) ;
#1298 = CARTESIAN_POINT ( 'NONE',  ( -18.73663160323380339, -9.000000000000003553, 5.000000000000079936 ) ) ;
#1299 = CARTESIAN_POINT ( 'NONE',  ( 3.355112389629172576, -2.681727112203168950, -0.2256878752776777242 ) ) ;
#1300 = AXIS2_PLACEMENT_3D ( 'NONE', #4873, #10299, #6568 ) ;
#1301 =( BOUNDED_CURVE ( )  B_SPLINE_CURVE ( 2, ( #8573, #11827, #14083, #4487, #6656, #23044, #12176, #888, #15541 ),
 .UNSPECIFIED., .F., .F. ) 
 B_SPLINE_CURVE_WITH_KNOTS ( ( 3, 2, 2, 2, 3 ),
 ( 0.7499999999999997780, 0.7656249999999996669, 0.7812499999999995559, 0.7968749999999994449, 0.8124999999999993339 ),
 .UNSPECIFIED. ) 
 CURVE ( )  GEOMETRIC_REPRESENTATION_ITEM ( )  RATIONAL_B_SPLINE_CURVE ( ( 1.000000000000001110, 0.9238795325112856283, 1.000000000000000000, 0.9238795325112867385, 1.000000000000000000, 0.9238795325112867385, 1.000000000000000000, 0.9238795325112899581, 0.9999999999999967804 ) ) 
 REPRESENTATION_ITEM ( '' )  );
#1302 = ADVANCED_FACE ( 'NONE', ( #23641 ), #156, .F. ) ;
#1303 = ORIENTED_EDGE ( 'NONE', *, *, #18011, .F. ) ;
#1304 = DIRECTION ( 'NONE',  ( 1.000000000000000000, -0.000000000000000000, -0.000000000000000000 ) ) ;
#1305 = ORIENTED_EDGE ( 'NONE', *, *, #8806, .T. ) ;
#1306 = EDGE_CURVE ( 'NONE', #20599, #22213, #19763, .T. ) ;
#1307 = DIRECTION ( 'NONE',  ( -0.3420201433256622181, 0.9396926207859106484, 1.232595164407828100E-31 ) ) ;
#1308 = ORIENTED_EDGE ( 'NONE', *, *, #15835, .T. ) ;
#1309 = CARTESIAN_POINT ( 'NONE',  ( 1.872352939448454495E-15, -3.458734125000000770, 11.93750000136560629 ) ) ;
#1310 = CARTESIAN_POINT ( 'NONE',  ( 51.18750000000000711, 9.999999999999989342, 11.99999999999999467 ) ) ;
#1311 = CARTESIAN_POINT ( 'NONE',  ( -65.85000000109248219, 7.933012699999995476, 14.99999999999999645 ) ) ;
#1312 = CARTESIAN_POINT ( 'NONE',  ( 67.00000000109247367, 12.06698729999999919, 14.14382582708705094 ) ) ;
#1313 = DIRECTION ( 'NONE',  ( 1.000000000000000000, 0.000000000000000000, 0.000000000000000000 ) ) ;
#1314 = VECTOR ( 'NONE', #157, 999.9999999999997726 ) ;
#1315 = CARTESIAN_POINT ( 'NONE',  ( -69.34999999999999432, 8.964466094067258695, 17.50000000000000355 ) ) ;
#1316 = AXIS2_PLACEMENT_3D ( 'NONE', #8399, #23094, #6705 ) ;
#1317 = CYLINDRICAL_SURFACE ( 'NONE', #10700, 4.250000000000000000 ) ;
#1318 = DIRECTION ( 'NONE',  ( -0.000000000000000000, -0.000000000000000000, -1.000000000000000000 ) ) ;
#1319 = CARTESIAN_POINT ( 'NONE',  ( 2.445694354108820079, 2.445694354108820523, 1.612500001365596125 ) ) ;
#1320 = DIRECTION ( 'NONE',  ( 1.224646799147353207E-16, -0.000000000000000000, 1.000000000000000000 ) ) ;
#1321 = EDGE_CURVE ( 'NONE', #12867, #6822, #20025, .T. ) ;
#1322 = CARTESIAN_POINT ( 'NONE',  ( -1.489200000000000079, 8.279592079675421725E-16, 6.760799999999997034 ) ) ;
#1323 = CARTESIAN_POINT ( 'NONE',  ( 3.458734125000002102, -1.432654583217639610, 17.87500000136560274 ) ) ;
#1324 = CARTESIAN_POINT ( 'NONE',  ( -10.13078668033273999, -11.25000000000000355, 5.000000000000079936 ) ) ;
#1325 = VERTEX_POINT ( 'NONE', #18370 ) ;
#1326 = CARTESIAN_POINT ( 'NONE',  ( 4.000000000000000000, 4.898587196589412829E-16, -3.074999997268812901 ) ) ;
#1327 = ORIENTED_EDGE ( 'NONE', *, *, #6855, .T. ) ;
#1328 = CARTESIAN_POINT ( 'NONE',  ( 54.52893183416158962, 11.17458954617365663, 18.02818770551464311 ) ) ;
#1329 = CARTESIAN_POINT ( 'NONE',  ( -68.40000000109249356, 9.143825827087050939, 12.93301269999999370 ) ) ;
#1330 = DIRECTION ( 'NONE',  ( 6.123233995736766036E-17, 1.000000000000000000, 0.000000000000000000 ) ) ;
#1331 = ADVANCED_FACE ( 'NONE', ( #7254 ), #1950, .F. ) ;
#1332 = DIRECTION ( 'NONE',  ( -0.000000000000000000, -1.000000000000000000, 0.000000000000000000 ) ) ;
#1333 = EDGE_LOOP ( 'NONE', ( #22696, #8411, #579, #16980 ) ) ;
#1334 = CYLINDRICAL_SURFACE ( 'NONE', #17915, 4.999999999999999112 ) ;
#1335 = EDGE_CURVE ( 'NONE', #10183, #22486, #22181, .T. ) ;
#1336 = AXIS2_PLACEMENT_3D ( 'NONE', #19570, #6898, #21593 ) ;
#1337 = ORIENTED_EDGE ( 'NONE', *, *, #14917, .F. ) ;
#1338 = CIRCLE ( 'NONE', #14763, 8.749000000000000554 ) ;
#1339 = CARTESIAN_POINT ( 'NONE',  ( 4.999999999999999112, -4.472189673936728838, -8.264486777890155622 ) ) ;
#1340 = EDGE_LOOP ( 'NONE', ( #18060, #5958, #5413, #5040 ) ) ;
#1341 = CARTESIAN_POINT ( 'NONE',  ( 50.65856816583843880, 6.028187705514649330, 16.72490539043803182 ) ) ;
#1342 = CARTESIAN_POINT ( 'NONE',  ( -68.65000000218496723, 8.964466094067258695, 17.50000000000000355 ) ) ;
#1343 = DIRECTION ( 'NONE',  ( 0.000000000000000000, 0.000000000000000000, -1.000000000000000000 ) ) ;
#1344 =( REPRESENTATION_RELATIONSHIP ('NONE','NONE', #8403, #9307 ) REPRESENTATION_RELATIONSHIP_WITH_TRANSFORMATION ( #11063 )SHAPE_REPRESENTATION_RELATIONSHIP( ) );
#1345 = CARTESIAN_POINT ( 'NONE',  ( -71.95000000109247651, 11.46158073645647235, 13.53841926354352232 ) ) ;
#1346 = CARTESIAN_POINT ( 'NONE',  ( -2.445694354108818303, -2.445694354108820967, 15.81250000136560629 ) ) ;
#1347 = CARTESIAN_POINT ( 'NONE',  ( 1.971781867644420635E-15, -4.000000000000000000, 11.37500000273119660 ) ) ;
#1348 = CARTESIAN_POINT ( 'NONE',  ( 59.15625000000002132, 7.000000000000003553, 16.24264068711929099 ) ) ;
#1349 = DIRECTION ( 'NONE',  ( 0.000000000000000000, 0.000000000000000000, 1.000000000000000000 ) ) ;
#1350 = AXIS2_PLACEMENT_3D ( 'NONE', #6037, #4242, #7493 ) ;
#1351 = CARTESIAN_POINT ( 'NONE',  ( 51.50231816583844591, 12.07320092032949610, 12.83056023321021044 ) ) ;
#1352 = VECTOR ( 'NONE', #12908, 1000.000000000000000 ) ;
#1353 = CARTESIAN_POINT ( 'NONE',  ( -1.432654583217640498, 3.458734125000000770, 0.8000000013655964581 ) ) ;
#1354 = CARTESIAN_POINT ( 'NONE',  ( -3.100354668897359112, -1.549725627487283042, 2.039999999999999591 ) ) ;
#1355 = CARTESIAN_POINT ( 'NONE',  ( 70.40000000218495302, 7.499999999999996447, 14.99999999999999645 ) ) ;
#1356 = B_SPLINE_CURVE_WITH_KNOTS ( 'NONE', 3,
 ( #20698, #2494, #3942, #7555, #20457, #16897 ),
 .UNSPECIFIED., .F., .F.,
 ( 4, 2, 4 ),
 ( 2.380733003178814001E-07, 0.001898835937927378101, 0.003797433802554438069 ),
 .UNSPECIFIED. ) ;
#1357 = VERTEX_POINT ( 'NONE', #22052 ) ;
#1358 = CARTESIAN_POINT ( 'NONE',  ( 0.000000000000000000, -7.593217523260523016, -7.958834565716849774 ) ) ;
#1359 = VERTEX_POINT ( 'NONE', #9523 ) ;
#1360 = CARTESIAN_POINT ( 'NONE',  ( 57.56250000000000000, 6.999999999999997335, 15.00000000000000533 ) ) ;
#1361 = CARTESIAN_POINT ( 'NONE',  ( -4.000000000000000000, 0.000000000000000000, -0.5749999972688123462 ) ) ;
#1362 = ADVANCED_FACE ( 'NONE', ( #1828 ), #9179, .T. ) ;
#1363 = LINE ( 'NONE', #18249, #21589 ) ;
#1364 = ORIENTED_EDGE ( 'NONE', *, *, #4274, .T. ) ;
#1365 = ORIENTED_EDGE ( 'NONE', *, *, #1794, .T. ) ;
#1366 = DIRECTION ( 'NONE',  ( 0.000000000000000000, 0.000000000000000000, 1.000000000000000000 ) ) ;
#1367 = DIRECTION ( 'NONE',  ( -1.000000000000000000, -7.703719777548943412E-32, 0.000000000000000000 ) ) ;
#1368 = ORIENTED_EDGE ( 'NONE', *, *, #10563, .T. ) ;
#1369 = DIRECTION ( 'NONE',  ( -1.000000000000000000, 0.000000000000000000, 0.000000000000000000 ) ) ;
#1370 = DIRECTION ( 'NONE',  ( 0.000000000000000000, 0.000000000000000000, -1.000000000000000000 ) ) ;
#1371 = CARTESIAN_POINT ( 'NONE',  ( 66.00000000109247367, 9.143825827087050939, 12.93301269999999370 ) ) ;
#1372 = CARTESIAN_POINT ( 'NONE',  ( 71.70000000000000284, 9.999999999999998224, 17.49999999999999645 ) ) ;
#1373 = CARTESIAN_POINT ( 'NONE',  ( -65.60000000218495586, 7.499999999999996447, 14.99999999999999645 ) ) ;
#1374 = CARTESIAN_POINT ( 'NONE',  ( 1.799999999999996048, 1.102182119232620869E-15, 9.000000000000023093 ) ) ;
#1375 = CARTESIAN_POINT ( 'NONE',  ( 56.93981816583843170, 10.06805114094564857, 19.00000000000000000 ) ) ;
#1376 = CARTESIAN_POINT ( 'NONE',  ( -2.445694354108820523, 2.445694354108820523, 2.612500001365597235 ) ) ;
#1377 = CARTESIAN_POINT ( 'NONE',  ( 1.432654583217643163, -3.458734124999999437, 15.75000000136560629 ) ) ;
#1378 = LINE ( 'NONE', #19478, #2861 ) ;
#1379 = LINE ( 'NONE', #7284, #5572 ) ;
#1380 = EDGE_LOOP ( 'NONE', ( #22643, #4683, #7458, #15884 ) ) ;
#1381 = LINE ( 'NONE', #12443, #16840 ) ;
#1382 = PLANE ( 'NONE',  #19705 ) ;
#1383 = FACE_OUTER_BOUND ( 'NONE', #10306, .T. ) ;
#1384 = VERTEX_POINT ( 'NONE', #17980 ) ;
#1385 = LINE ( 'NONE', #3315, #2950 ) ;
#1386 = CARTESIAN_POINT ( 'NONE',  ( 3.263761790716562139, -8.974600000000002353, 5.000000000000079936 ) ) ;
#1387 = CARTESIAN_POINT ( 'NONE',  ( 59.34375000000000711, 8.343145750507636293, 19.00000000000000000 ) ) ;
#1388 = ORIENTED_EDGE ( 'NONE', *, *, #19640, .T. ) ;
#1389 = DIRECTION ( 'NONE',  ( 1.000000000000000000, 7.703719777548943412E-32, 0.000000000000000000 ) ) ;
#1390 = ORIENTED_EDGE ( 'NONE', *, *, #6277, .F. ) ;
#1391 = CARTESIAN_POINT ( 'NONE',  ( 57.68981816583843170, 9.931948859054346102, 10.99999999999999467 ) ) ;
#1392 = CARTESIAN_POINT ( 'NONE',  ( 68.95000000218495018, 8.964466094067258695, 12.49999999999999289 ) ) ;
#1393 = EDGE_CURVE ( 'NONE', #22332, #19018, #22039, .T. ) ;
#1394 = CARTESIAN_POINT ( 'NONE',  ( 28.39650299071657003, -8.974600000000002353, 5.000000000000079936 ) ) ;
#1395 = CARTESIAN_POINT ( 'NONE',  ( -68.79999999999999716, 8.232233047033629347, 13.23223304703362402 ) ) ;
#1396 = CARTESIAN_POINT ( 'NONE',  ( -4.000000000000000000, 0.000000000000000000, -0.6999999999999975131 ) ) ;
#1397 = ORIENTED_EDGE ( 'NONE', *, *, #16708, .T. ) ;
#1398 = AXIS2_PLACEMENT_3D ( 'NONE', #703, #8039, #228 ) ;
#1399 = DIRECTION ( 'NONE',  ( -1.000000000000000000, -0.000000000000000000, 0.000000000000000000 ) ) ;
#1400 = PLANE ( 'NONE',  #4170 ) ;
#1401 = EDGE_CURVE ( 'NONE', #18845, #18467, #22431, .T. ) ;
#1402 = CARTESIAN_POINT ( 'NONE',  ( 68.00000000109245946, 12.06698730000000275, 14.14382582708705094 ) ) ;
#1403 = AXIS2_PLACEMENT_3D ( 'NONE', #21864, #5470, #16151 ) ;
#1404 = CARTESIAN_POINT ( 'NONE',  ( -2.445694354108818303, -2.445694354108820967, 17.81250000136560274 ) ) ;
#1405 = CARTESIAN_POINT ( 'NONE',  ( 72.50000000000000000, 9.999999999999998224, 14.99999999999999645 ) ) ;
#1406 = CIRCLE ( 'NONE', #7172, 0.5155456020628804703 ) ;
#1407 = DIRECTION ( 'NONE',  ( 1.000000000000000000, 0.000000000000000000, 0.000000000000000000 ) ) ;
#1408 = ORIENTED_EDGE ( 'NONE', *, *, #14798, .F. ) ;
#1409 = DIRECTION ( 'NONE',  ( 0.000000000000000000, 0.000000000000000000, -1.000000000000000000 ) ) ;
#1410 = CARTESIAN_POINT ( 'NONE',  ( 54.75000000000000711, 7.878679656440361612, 17.12132034355964549 ) ) ;
#1411 = CARTESIAN_POINT ( 'NONE',  ( 66.49999999999998579, 9.999999999999998224, 12.49999999999999289 ) ) ;
#1412 = ORIENTED_EDGE ( 'NONE', *, *, #20233, .F. ) ;
#1413 = FACE_OUTER_BOUND ( 'NONE', #7586, .T. ) ;
#1414 = CARTESIAN_POINT ( 'NONE',  ( 3.458734125000000326, 1.432654583217640498, -0.6999999986344048741 ) ) ;
#1415 = FACE_OUTER_BOUND ( 'NONE', #16177, .T. ) ;
#1416 = ORIENTED_EDGE ( 'NONE', *, *, #16738, .F. ) ;
#1417 = CARTESIAN_POINT ( 'NONE',  ( -66.05000000218494449, 12.50000000000000000, 16.03553390593273775 ) ) ;
#1418 = EDGE_LOOP ( 'NONE', ( #4713, #10059, #19395, #21066 ) ) ;
#1419 = CIRCLE ( 'NONE', #13308, 4.000000000000000888 ) ;
#1420 = FACE_OUTER_BOUND ( 'NONE', #1217, .T. ) ;
#1421 = ORIENTED_EDGE ( 'NONE', *, *, #7801, .T. ) ;
#1422 = B_SPLINE_CURVE_WITH_KNOTS ( 'NONE', 3,
 ( #8160, #15471, #15360, #2388, #16902, #18558, #22501, #13443 ),
 .UNSPECIFIED., .F., .F.,
 ( 4, 2, 2, 4 ),
 ( 0.003797433802554446743, 0.004743183970586241360, 0.005688934138618037713, 0.007580434474681626081 ),
 .UNSPECIFIED. ) ;
#1423 = CARTESIAN_POINT ( 'NONE',  ( -2.828427124746188515, -2.828427124746190735, 19.12500000000001066 ) ) ;
#1424 = CARTESIAN_POINT ( 'NONE',  ( -4.000000000000000000, 0.000000000000000000, 0.000000000000000000 ) ) ;
#1425 = CIRCLE ( 'NONE', #11801, 4.000000000000001776 ) ;
#1426 = AXIS2_PLACEMENT_3D ( 'NONE', #20889, #22335, #13514 ) ;
#1427 = EDGE_CURVE ( 'NONE', #12772, #21867, #14168, .T. ) ;
#1428 = CARTESIAN_POINT ( 'NONE',  ( -65.70000000109249072, 9.143825827087049163, 17.06698729999999742 ) ) ;
#1429 = EDGE_CURVE ( 'NONE', #8404, #10654, #11585, .T. ) ;
#1430 = CARTESIAN_POINT ( 'NONE',  ( 66.05000000109247082, 9.999999999999998224, 12.93301269999999192 ) ) ;
#1431 = DIRECTION ( 'NONE',  ( 1.224646799147353207E-16, -0.000000000000000000, 1.000000000000000000 ) ) ;
#1432 = CARTESIAN_POINT ( 'NONE',  ( -71.84999999999999432, 7.499999999999995559, 16.03553390593273420 ) ) ;
#1433 = LINE ( 'NONE', #8656, #7623 ) ;
#1434 = EDGE_CURVE ( 'NONE', #2153, #12123, #14043, .T. ) ;
#1435 = CARTESIAN_POINT ( 'NONE',  ( 60.00000000000002132, 13.28258829677531239, 17.07862169589594004 ) ) ;
#1436 = EDGE_CURVE ( 'NONE', #17091, #22338, #12550, .T. ) ;
#1437 = AXIS2_PLACEMENT_3D ( 'NONE', #12710, #14257, #21515 ) ;
#1438 =( BOUNDED_CURVE ( )  B_SPLINE_CURVE ( 2, ( #21050, #14260, #7310, #1530, #19966 ),
 .UNSPECIFIED., .F., .F. ) 
 B_SPLINE_CURVE_WITH_KNOTS ( ( 3, 2, 3 ),
 ( 0.9000000000000000222, 0.9124999999999999778, 0.9155333511103322941 ),
 .UNSPECIFIED. ) 
 CURVE ( )  GEOMETRIC_REPRESENTATION_ITEM ( )  RATIONAL_B_SPLINE_CURVE ( ( 1.000000000000000000, 0.9238795325112867385, 1.000000000000000000, 0.9815279916339278987, 0.9720211172018224932 ) ) 
 REPRESENTATION_ITEM ( '' )  );
#1439 = CARTESIAN_POINT ( 'NONE',  ( -2.445694354108820523, 2.445694354108820523, -2.137499998634403653 ) ) ;
#1440 = CARTESIAN_POINT ( 'NONE',  ( 67.40000000218495302, 9.999999999999998224, 12.49999999999999289 ) ) ;
#1441 = FACE_OUTER_BOUND ( 'NONE', #20684, .T. ) ;
#1442 = CARTESIAN_POINT ( 'NONE',  ( -1.432654583217638944, 3.458734125000000326, 17.25000000136560274 ) ) ;
#1443 = CARTESIAN_POINT ( 'NONE',  ( -66.60000000218495586, 9.999999999999998224, 12.49999999999999289 ) ) ;
#1444 = AXIS2_PLACEMENT_3D ( 'NONE', #22943, #17911, #1247 ) ;
#1445 = ORIENTED_EDGE ( 'NONE', *, *, #21073, .F. ) ;
#1446 = VECTOR ( 'NONE', #11096, 1000.000000000000000 ) ;
#1447 = CARTESIAN_POINT ( 'NONE',  ( -71.20000000109246230, 10.85617417291294551, 17.06698730000000097 ) ) ;
#1448 = EDGE_LOOP ( 'NONE', ( #14635, #6191, #18723, #16969 ) ) ;
#1449 = CARTESIAN_POINT ( 'NONE',  ( 54.15393183416158251, 6.971812294485357775, 16.17458954617365663 ) ) ;
#1450 = CARTESIAN_POINT ( 'NONE',  ( -68.55000000109247082, 11.46158073645647235, 13.53841926354352232 ) ) ;
#1451 = MECHANICAL_DESIGN_GEOMETRIC_PRESENTATION_REPRESENTATION (  '', ( #20581 ), #7598 ) ;
#1452 = CARTESIAN_POINT ( 'NONE',  ( -3.458734125000000326, 1.432654583217640276, -2.324999998634404097 ) ) ;
#1453 = ORIENTED_EDGE ( 'NONE', *, *, #3608, .F. ) ;
#1454 = CYLINDRICAL_SURFACE ( 'NONE', #22857, 2.500000000000000444 ) ;
#1455 = EDGE_CURVE ( 'NONE', #6574, #22213, #5240, .T. ) ;
#1456 = ORIENTED_EDGE ( 'NONE', *, *, #8400, .F. ) ;
#1457 = CARTESIAN_POINT ( 'NONE',  ( 0.000000000000000000, 0.4999240074894452657, 8.734705317681628500 ) ) ;
#1458 = ORIENTED_EDGE ( 'NONE', *, *, #22694, .F. ) ;
#1459 = CARTESIAN_POINT ( 'NONE',  ( 51.12731816583844591, 12.16943976678978601, 17.07320092032949432 ) ) ;
#1460 = AXIS2_PLACEMENT_3D ( 'NONE', #4182, #2261, #11163 ) ;
#1461 = CARTESIAN_POINT ( 'NONE',  ( -68.00000000218494733, 7.499999999999996447, 14.99999999999999645 ) ) ;
#1462 = EDGE_CURVE ( 'NONE', #20146, #12336, #3240, .T. ) ;
#1463 = DIRECTION ( 'NONE',  ( -0.3420201433256622181, 0.9396926207859106484, 1.232595164407828100E-31 ) ) ;
#1464 = CARTESIAN_POINT ( 'NONE',  ( 20.00000000000000000, 1.500000000000003109, -17.32050807568893092 ) ) ;
#1465 = CIRCLE ( 'NONE', #16418, 2.649999999999992806 ) ;
#1466 = CARTESIAN_POINT ( 'NONE',  ( 1.432654583217641386, 3.458734125000000770, 15.37500000136560807 ) ) ;
#1467 = DIRECTION ( 'NONE',  ( -1.000000000000000000, 0.000000000000000000, 0.000000000000000000 ) ) ;
#1468 = EDGE_CURVE ( 'NONE', #20225, #9434, #3125, .T. ) ;
#1469 = CARTESIAN_POINT ( 'NONE',  ( 56.81250000000000000, 13.00000000000000000, 14.99999999999998757 ) ) ;
#1470 = CARTESIAN_POINT ( 'NONE',  ( 67.20000000000000284, 8.232233047033629347, 13.23223304703362402 ) ) ;
#1471 = EDGE_CURVE ( 'NONE', #16384, #8981, #8772, .T. ) ;
#1472 = CARTESIAN_POINT ( 'NONE',  ( 50.18981816583844591, 9.931948859054354983, 11.99999999999999645 ) ) ;
#1473 = CARTESIAN_POINT ( 'NONE',  ( -3.458734125000000770, 0.000000000000000000, 1.987500001365596569 ) ) ;
#1474 = CARTESIAN_POINT ( 'NONE',  ( -1.914603566986515348, -2.889253230644202031, 2.039999999999998703 ) ) ;
#1475 = AXIS2_PLACEMENT_3D ( 'NONE', #8775, #10591, #19885 ) ;
#1476 = CARTESIAN_POINT ( 'NONE',  ( 2.000000000000001776, 0.000000000000000000, 0.000000000000000000 ) ) ;
#1477 = VECTOR ( 'NONE', #3706, 1000.000000000000000 ) ;
#1478 = VERTEX_POINT ( 'NONE', #10701 ) ;
#1479 = CARTESIAN_POINT ( 'NONE',  ( -90.00000000000000000, 0.000000000000000000, 0.000000000000000000 ) ) ;
#1480 = CARTESIAN_POINT ( 'NONE',  ( -2.756197834950067094, -3.027510591568735254, -3.223146290109809797 ) ) ;
#1481 = ORIENTED_EDGE ( 'NONE', *, *, #22334, .F. ) ;
#1482 = CARTESIAN_POINT ( 'NONE',  ( 59.15625000000002132, 7.000000000000003553, 16.24264068711929099 ) ) ;
#1483 = CARTESIAN_POINT ( 'NONE',  ( -4.000000000000000000, -1.656854249492383246, 1.487500002731187543 ) ) ;
#1484 = DIRECTION ( 'NONE',  ( 0.3420201433256622736, -0.9396926207859106484, -1.232595164407828100E-31 ) ) ;
#1485 = ORIENTED_EDGE ( 'NONE', *, *, #10165, .T. ) ;
#1486 = AXIS2_PLACEMENT_3D ( 'NONE', #8670, #15968, #10604 ) ;
#1487 = CARTESIAN_POINT ( 'NONE',  ( -2.828427124746188515, -2.828427124746190735, 19.12500000000001066 ) ) ;
#1488 = EDGE_LOOP ( 'NONE', ( #20968, #10757, #16555, #15110 ) ) ;
#1489 =( BOUNDED_CURVE ( )  B_SPLINE_CURVE ( 2, ( #9941, #22479, #9817, #5972, #17238, #4406, #20909, #686, #6333 ),
 .UNSPECIFIED., .F., .F. ) 
 B_SPLINE_CURVE_WITH_KNOTS ( ( 3, 2, 2, 2, 3 ),
 ( 0.2500000000000006661, 0.2656250000000005551, 0.2812500000000004441, 0.2968750000000003886, 0.3125000000000002776 ),
 .UNSPECIFIED. ) 
 CURVE ( )  GEOMETRIC_REPRESENTATION_ITEM ( )  RATIONAL_B_SPLINE_CURVE ( ( 0.9999999999999967804, 0.9238795325112899581, 1.000000000000000000, 0.9238795325112867385, 1.000000000000000000, 0.9238795325112867385, 1.000000000000000000, 0.9238795325112854062, 1.000000000000001332 ) ) 
 REPRESENTATION_ITEM ( '' )  );
#1490 = LINE ( 'NONE', #8831, #18279 ) ;
#1491 = AXIS2_PLACEMENT_3D ( 'NONE', #19343, #17798, #1369 ) ;
#1492 = CARTESIAN_POINT ( 'NONE',  ( 0.000000000000000000, 0.000000000000000000, -4.000000000000000000 ) ) ;
#1493 = ORIENTED_EDGE ( 'NONE', *, *, #3803, .T. ) ;
#1494 = CARTESIAN_POINT ( 'NONE',  ( -15.00000000000000711, 10.00000000000000000, -19.99999999999999645 ) ) ;
#1495 = APPLICATION_CONTEXT ( 'automotive_design' ) ;
#1496 = CARTESIAN_POINT ( 'NONE',  ( -2.828427124746188515, -2.828427124746190735, 11.12500000000001066 ) ) ;
#1497 = ORIENTED_EDGE ( 'NONE', *, *, #22701, .T. ) ;
#1498 = CIRCLE ( 'NONE', #10721, 2.499999999999998668 ) ;
#1499 = CARTESIAN_POINT ( 'NONE',  ( 0.000000000000000000, 0.000000000000000000, 2.039999999999998259 ) ) ;
#1500 = CIRCLE ( 'NONE', #7252, 4.999999999999997335 ) ;
#1501 = CARTESIAN_POINT ( 'NONE',  ( 71.00000000000000000, 8.232233047033627571, 16.76776695296636532 ) ) ;
#1502 = EDGE_CURVE ( 'NONE', #11449, #21785, #7339, .T. ) ;
#1503 = CARTESIAN_POINT ( 'NONE',  ( 1.236993788156008760E-15, 0.000000000000000000, 21.31370849898476649 ) ) ;
#1504 = EDGE_CURVE ( 'NONE', #10342, #4211, #2172, .T. ) ;
#1505 = DIRECTION ( 'NONE',  ( 1.224646799147353207E-16, -0.000000000000000000, 1.000000000000000000 ) ) ;
#1506 = CIRCLE ( 'NONE', #5720, 2.500000000000000888 ) ;
#1507 = CARTESIAN_POINT ( 'NONE',  ( 51.84375000000001421, 8.343145750507638070, 19.00000000000000711 ) ) ;
#1508 = CARTESIAN_POINT ( 'NONE',  ( 2.445694354108820079, 2.445694354108820523, 4.362500001365595459 ) ) ;
#1509 = CARTESIAN_POINT ( 'NONE',  ( -1.432654583217638944, 3.458734125000000326, 15.25000000136560807 ) ) ;
#1510 = CARTESIAN_POINT ( 'NONE',  ( -2.449293598294706907E-16, 4.000000000000000000, 0.05000000000000143219 ) ) ;
#1511 = DIRECTION ( 'NONE',  ( -1.000000000000000000, 0.000000000000000000, 0.000000000000000000 ) ) ;
#1512 = EDGE_LOOP ( 'NONE', ( #7438, #8198, #13441, #21564, #11897, #1337 ) ) ;
#1513 = CARTESIAN_POINT ( 'NONE',  ( 4.999999999999999112, 8.475820894093034852, -4.057423117305300586 ) ) ;
#1514 = DIRECTION ( 'NONE',  ( 1.000000000000000000, 4.625929269271486900E-16, 0.000000000000000000 ) ) ;
#1515 = FACE_OUTER_BOUND ( 'NONE', #19754, .T. ) ;
#1516 = ORIENTED_EDGE ( 'NONE', *, *, #9390, .T. ) ;
#1517 = CIRCLE ( 'NONE', #19859, 8.749000000000000554 ) ;
#1518 = CARTESIAN_POINT ( 'NONE',  ( 2.828427124746191179, 2.828427124746190291, 13.75000000273119483 ) ) ;
#1519 = CARTESIAN_POINT ( 'NONE',  ( 4.999999999999999112, 0.000000000000000000, 0.000000000000000000 ) ) ;
#1520 = ORIENTED_EDGE ( 'NONE', *, *, #23567, .F. ) ;
#1521 = CARTESIAN_POINT ( 'NONE',  ( 4.999999999999999112, 0.000000000000000000, 0.000000000000000000 ) ) ;
#1522 = ORIENTED_EDGE ( 'NONE', *, *, #14669, .T. ) ;
#1523 = CARTESIAN_POINT ( 'NONE',  ( 58.81481816583843170, 14.00000000000000178, 14.93194885905434610 ) ) ;
#1524 = CIRCLE ( 'NONE', #13801, 4.000000000000000000 ) ;
#1525 = CARTESIAN_POINT ( 'NONE',  ( 67.85000000218495586, 8.964466094067258695, 17.50000000000000355 ) ) ;
#1526 = DIRECTION ( 'NONE',  ( -1.000000000000000000, -0.000000000000000000, -0.000000000000000000 ) ) ;
#1527 = DIRECTION ( 'NONE',  ( -1.000000000000000000, -6.123233995736827666E-17, 0.000000000000000000 ) ) ;
#1528 = DIRECTION ( 'NONE',  ( -1.224646799147353207E-16, 0.000000000000000000, -1.000000000000000000 ) ) ;
#1529 = ORIENTED_EDGE ( 'NONE', *, *, #19125, .F. ) ;
#1530 = CARTESIAN_POINT ( 'NONE',  ( -2.560821871666743910, 3.096032377825634896, 9.985724042037038117 ) ) ;
#1531 = CARTESIAN_POINT ( 'NONE',  ( 52.93518183416157541, 9.931948859054372747, 17.99999999999999645 ) ) ;
#1532 = CARTESIAN_POINT ( 'NONE',  ( 22.70968385928345157, -8.974600000000002353, 5.000000000000079936 ) ) ;
#1533 = CARTESIAN_POINT ( 'NONE',  ( 67.20000000109247651, 12.06698730000000275, 14.14382582708705094 ) ) ;
#1534 = CARTESIAN_POINT ( 'NONE',  ( -3.458734124999998993, 0.000000000000000000, 10.43750000136560452 ) ) ;
#1535 = AXIS2_PLACEMENT_3D ( 'NONE', #11276, #20220, #18550 ) ;
#1536 = CARTESIAN_POINT ( 'NONE',  ( -68.05000000000001137, 8.964466094067256918, 12.49999999999999822 ) ) ;
#1537 = DIRECTION ( 'NONE',  ( 0.000000000000000000, -0.8090169943749403458, -0.5877852522924831291 ) ) ;
#1538 = ORIENTED_EDGE ( 'NONE', *, *, #1994, .F. ) ;
#1539 = CARTESIAN_POINT ( 'NONE',  ( 2.499999999999999556, 4.762163868918413812, -9.915734732513168836 ) ) ;
#1540 = CARTESIAN_POINT ( 'NONE',  ( 59.53125000000000711, 11.24264068711929276, 18.00000000000000000 ) ) ;
#1541 = CARTESIAN_POINT ( 'NONE',  ( 1.656854249492381470, 4.000000000000000000, 10.81250000273119660 ) ) ;
#1542 =( NAMED_UNIT ( * ) PLANE_ANGLE_UNIT ( ) SI_UNIT ( $, .RADIAN. ) );
#1543 = VERTEX_POINT ( 'NONE', #7216 ) ;
#1544 = EDGE_CURVE ( 'NONE', #8315, #18533, #3361, .T. ) ;
#1545 = FACE_OUTER_BOUND ( 'NONE', #5338, .T. ) ;
#1546 = CARTESIAN_POINT ( 'NONE',  ( 2.445694354108820079, 2.445694354108820523, -0.6374999986344040970 ) ) ;
#1547 = CARTESIAN_POINT ( 'NONE',  ( 31.53809564071656624, -8.974600000000002353, 10.00000000000008882 ) ) ;
#1548 = ORIENTED_EDGE ( 'NONE', *, *, #21156, .T. ) ;
#1549 = CYLINDRICAL_SURFACE ( 'NONE', #18581, 11.00000000000000000 ) ;
#1550 = VERTEX_POINT ( 'NONE', #8895 ) ;
#1551 = CARTESIAN_POINT ( 'NONE',  ( -3.999999999999999112, 1.656854249492380582, 18.93750000000001066 ) ) ;
#1552 = CARTESIAN_POINT ( 'NONE',  ( 9.920644283265380691E-16, 4.000000000000000000, 18.75000000000001066 ) ) ;
#1553 = CARTESIAN_POINT ( 'NONE',  ( 5.560781378645573980, 6.809993116116507654E-16, -4.000000000000000000 ) ) ;
#1554 = CIRCLE ( 'NONE', #3866, 0.1999999999999996503 ) ;
#1555 = B_SPLINE_CURVE_WITH_KNOTS ( 'NONE', 3,
 ( #21035, #4761, #12096, #11981, #19248, #2836, #17596, #19361 ),
 .UNSPECIFIED., .F., .F.,
 ( 4, 2, 2, 4 ),
 ( 0.000000000000000000, 0.002450665683189819262, 0.003675998524784728893, 0.004901331366379639391 ),
 .UNSPECIFIED. ) ;
#1556 = FACE_OUTER_BOUND ( 'NONE', #21064, .T. ) ;
#1557 = CARTESIAN_POINT ( 'NONE',  ( 0.000000000000000000, 0.000000000000000000, 0.000000000000000000 ) ) ;
#1558 = DIRECTION ( 'NONE',  ( 0.000000000000000000, 0.000000000000000000, 1.000000000000000000 ) ) ;
#1559 = CARTESIAN_POINT ( 'NONE',  ( -68.25000000000000000, 12.50000000000000000, 13.96446609406725869 ) ) ;
#1560 = LINE ( 'NONE', #9021, #16034 ) ;
#1561 = DIRECTION ( 'NONE',  ( -1.000000000000000000, 0.000000000000000000, 0.000000000000000000 ) ) ;
#1562 = DIRECTION ( 'NONE',  ( 0.000000000000000000, 0.5877852522924743583, -0.8090169943749467851 ) ) ;
#1563 = CARTESIAN_POINT ( 'NONE',  ( 2.445694354108820079, 2.445694354108820523, -0.3874999986344038194 ) ) ;
#1564 = DIRECTION ( 'NONE',  ( 0.3420201433256622181, -0.9396926207859107594, 0.000000000000000000 ) ) ;
#1565 = CARTESIAN_POINT ( 'NONE',  ( 4.999999999999999112, 0.000000000000000000, 0.000000000000000000 ) ) ;
#1566 = CARTESIAN_POINT ( 'NONE',  ( 1.025207404391860050E-15, 3.458734125000000326, 18.18750000136560274 ) ) ;
#1567 = DIRECTION ( 'NONE',  ( 0.000000000000000000, 0.000000000000000000, 1.000000000000000000 ) ) ;
#1568 = ORIENTED_EDGE ( 'NONE', *, *, #14803, .T. ) ;
#1569 = ADVANCED_FACE ( 'NONE', ( #21794 ), #6968, .T. ) ;
#1570 = CARTESIAN_POINT ( 'NONE',  ( -71.85000000109246798, 12.06698730000000097, 14.99999999999999645 ) ) ;
#1571 = ORIENTED_EDGE ( 'NONE', *, *, #13112, .T. ) ;
#1572 = CARTESIAN_POINT ( 'NONE',  ( 56.21643183416158251, 13.97181229448536399, 16.72490539043799629 ) ) ;
#1573 = CARTESIAN_POINT ( 'NONE',  ( -66.90000000109246514, 10.85617417291294551, 12.93301269999999370 ) ) ;
#1574 = DIRECTION ( 'NONE',  ( 0.000000000000000000, 0.000000000000000000, -1.000000000000000000 ) ) ;
#1575 = ADVANCED_FACE ( 'NONE', ( #3592 ), #21669, .T. ) ;
#1576 = CARTESIAN_POINT ( 'NONE',  ( 1.432654583217642053, -3.458734124999999437, -2.949999998634404985 ) ) ;
#1577 = ORIENTED_EDGE ( 'NONE', *, *, #12655, .F. ) ;
#1578 = CARTESIAN_POINT ( 'NONE',  ( -18.34148624732256394, -8.396350360904289545, 10.00000000000008882 ) ) ;
#1579 = ORIENTED_EDGE ( 'NONE', *, *, #22022, .F. ) ;
#1580 = DIRECTION ( 'NONE',  ( 0.000000000000000000, 0.000000000000000000, 1.000000000000000000 ) ) ;
#1581 = EDGE_LOOP ( 'NONE', ( #527, #11428, #15379, #1485 ) ) ;
#1582 = ADVANCED_FACE ( 'NONE', ( #23477 ), #14407, .F. ) ;
#1583 = CARTESIAN_POINT ( 'NONE',  ( 59.62500000000000711, 12.12132034355964727, 17.12132034355963484 ) ) ;
#1584 = CARTESIAN_POINT ( 'NONE',  ( -71.30000000109248504, 9.143825827087049163, 17.06698729999999742 ) ) ;
#1585 = CARTESIAN_POINT ( 'NONE',  ( -20.00000000000001066, 4.500000000000003553, -50.00000000000000000 ) ) ;
#1586 = CARTESIAN_POINT ( 'NONE',  ( 21.00000000000000355, 0.000000000000000000, 0.000000000000000000 ) ) ;
#1587 =( BOUNDED_CURVE ( )  B_SPLINE_CURVE ( 2, ( #22498, #7559, #22375, #11170, #13439, #18441, #9361, #18802, #14881 ),
 .UNSPECIFIED., .F., .F. ) 
 B_SPLINE_CURVE_WITH_KNOTS ( ( 3, 2, 2, 2, 3 ),
 ( 0.1000000000000000056, 0.1125000000000000028, 0.1250000000000000000, 0.1375000000000000111, 0.1499999999999999944 ),
 .UNSPECIFIED. ) 
 CURVE ( )  GEOMETRIC_REPRESENTATION_ITEM ( )  RATIONAL_B_SPLINE_CURVE ( ( 1.000000000000000000, 0.9238795325112867385, 1.000000000000000000, 0.9238795325112867385, 1.000000000000000000, 0.9238795325112867385, 1.000000000000000000, 0.9238795325112867385, 1.000000000000000000 ) ) 
 REPRESENTATION_ITEM ( '' )  );
#1588 = CARTESIAN_POINT ( 'NONE',  ( 3.458734125000001658, 1.432654583217640498, 16.25000000136560629 ) ) ;
#1589 = CARTESIAN_POINT ( 'NONE',  ( -4.000000000000000000, 0.000000000000000000, -2.574999997268812457 ) ) ;
#1590 = CARTESIAN_POINT ( 'NONE',  ( 54.65625000000001421, 7.000000000000003553, 16.24264068711929099 ) ) ;
#1591 = CARTESIAN_POINT ( 'NONE',  ( 72.50000000000000000, 9.999999999999998224, 17.49999999999999645 ) ) ;
#1592 = CARTESIAN_POINT ( 'NONE',  ( 59.15625000000002132, 7.000000000000003553, 16.24264068711929099 ) ) ;
#1593 = EDGE_CURVE ( 'NONE', #17904, #18669, #255, .T. ) ;
#1594 = CARTESIAN_POINT ( 'NONE',  ( 1.432654583217640276, 3.458734125000000770, -2.324999998634404097 ) ) ;
#1595 = CARTESIAN_POINT ( 'NONE',  ( -2.872501113216805901, -1.939738628788093999, 2.039999999999998703 ) ) ;
#1596 = CARTESIAN_POINT ( 'NONE',  ( 4.999999999999999112, 5.222868219166856285, 9.680994141368790551 ) ) ;
#1597 = VERTEX_POINT ( 'NONE', #3516 ) ;
#1598 = CARTESIAN_POINT ( 'NONE',  ( 70.45000000000000284, 8.964466094067244484, 12.50000000000000711 ) ) ;
#1599 = DIRECTION ( 'NONE',  ( -0.000000000000000000, -0.000000000000000000, 1.000000000000000000 ) ) ;
#1600 = ORIENTED_EDGE ( 'NONE', *, *, #1015, .T. ) ;
#1601 = CARTESIAN_POINT ( 'NONE',  ( 55.50000000000000711, 12.12132034355963484, 12.87867965644034740 ) ) ;
#1602 = CARTESIAN_POINT ( 'NONE',  ( -1.656854249492381248, -3.999999999999999112, -0.3874999972688123462 ) ) ;
#1603 = EDGE_CURVE ( 'NONE', #13238, #7689, #17892, .T. ) ;
#1604 = DIRECTION ( 'NONE',  ( -1.000000000000000000, -0.000000000000000000, -0.000000000000000000 ) ) ;
#1605 = ORIENTED_EDGE ( 'NONE', *, *, #16420, .T. ) ;
#1606 = CARTESIAN_POINT ( 'NONE',  ( -1.656854249492380138, -3.999999999999999112, 17.18750000000001066 ) ) ;
#1607 = ORIENTED_EDGE ( 'NONE', *, *, #11431, .F. ) ;
#1608 = DIRECTION ( 'NONE',  ( 1.000000000000000000, 0.000000000000000000, 0.000000000000000000 ) ) ;
#1609 = EDGE_LOOP ( 'NONE', ( #3684, #17235, #21402, #18937 ) ) ;
#1610 = ADVANCED_FACE ( 'NONE', ( #19439 ), #4963, .F. ) ;
#1611 = CARTESIAN_POINT ( 'NONE',  ( 0.000000000000000000, -3.174628368996021521, -8.152713396088794084 ) ) ;
#1612 = EDGE_CURVE ( 'NONE', #7519, #14091, #3168, .T. ) ;
#1613 = CARTESIAN_POINT ( 'NONE',  ( -2.828427124746189403, 2.828427124746190291, 11.87500000000001066 ) ) ;
#1614 = EDGE_LOOP ( 'NONE', ( #12666, #11057, #5802 ) ) ;
#1615 = CARTESIAN_POINT ( 'NONE',  ( 65.80000000109247082, 7.933012699999995476, 15.85617417291294196 ) ) ;
#1616 = CARTESIAN_POINT ( 'NONE',  ( 66.20000000109246230, 9.143825827087050939, 12.93301269999999370 ) ) ;
#1617 = VECTOR ( 'NONE', #1156, 1000.000000000000000 ) ;
#1618 = LINE ( 'NONE', #7150, #16240 ) ;
#1619 = CIRCLE ( 'NONE', #15049, 4.000000000000001776 ) ;
#1620 = CARTESIAN_POINT ( 'NONE',  ( 69.55000000218493028, 7.499999999999996447, 16.03553390593273775 ) ) ;
#1621 = CARTESIAN_POINT ( 'NONE',  ( 56.37731816583843170, 7.123453452023657206, 12.21969229848395599 ) ) ;
#1622 = CARTESIAN_POINT ( 'NONE',  ( -2.445694354108820523, 2.445694354108820523, 1.612500001365596125 ) ) ;
#1623 = CARTESIAN_POINT ( 'NONE',  ( 0.000000000000000000, -7.360373001730951437, 4.729683950898845524 ) ) ;
#1624 = CARTESIAN_POINT ( 'NONE',  ( -3.458734124999998993, 0.000000000000000000, 14.43750000136560452 ) ) ;
#1625 = CARTESIAN_POINT ( 'NONE',  ( 72.50000000000000000, 9.999999999999998224, 14.99999999999999645 ) ) ;
#1626 = CARTESIAN_POINT ( 'NONE',  ( -65.00000000000000000, 9.999999999999998224, 25.00000000000001421 ) ) ;
#1627 = EDGE_LOOP ( 'NONE', ( #4407, #12067, #3715, #23565 ) ) ;
#1628 = DIRECTION ( 'NONE',  ( 1.000000000000000000, -0.000000000000000000, -0.000000000000000000 ) ) ;
#1629 = LINE ( 'NONE', #8603, #18204 ) ;
#1630 = CARTESIAN_POINT ( 'NONE',  ( 65.00000000000000000, 15.00000000000000000, 10.00000000000007105 ) ) ;
#1631 = VERTEX_POINT ( 'NONE', #19559 ) ;
#1632 = VERTEX_POINT ( 'NONE', #14203 ) ;
#1633 = LINE ( 'NONE', #12448, #22458 ) ;
#1634 = ADVANCED_FACE ( 'NONE', ( #14436 ), #8929, .T. ) ;
#1635 = EDGE_CURVE ( 'NONE', #7935, #14210, #23634, .T. ) ;
#1636 = CYLINDRICAL_SURFACE ( 'NONE', #20929, 8.749000000000002331 ) ;
#1637 = EDGE_LOOP ( 'NONE', ( #4447, #2835 ) ) ;
#1638 = DIRECTION ( 'NONE',  ( 1.000000000000000000, 0.000000000000000000, 0.000000000000000000 ) ) ;
#1639 = ORIENTED_EDGE ( 'NONE', *, *, #904, .F. ) ;
#1640 = ADVANCED_FACE ( 'NONE', ( #9048 ), #14563, .T. ) ;
#1641 = CARTESIAN_POINT ( 'NONE',  ( 53.62500000000000711, 12.82842712474620228, 17.82842712474617386 ) ) ;
#1642 = CIRCLE ( 'NONE', #2024, 0.2000000000000005107 ) ;
#1643 = CARTESIAN_POINT ( 'NONE',  ( 66.55000000218494449, 8.964466094067258695, 12.49999999999999289 ) ) ;
#1644 = DIRECTION ( 'NONE',  ( 0.000000000000000000, 0.000000000000000000, -1.000000000000000000 ) ) ;
#1645 = DIRECTION ( 'NONE',  ( 0.000000000000000000, -0.9510565162951499785, -0.3090169943749581649 ) ) ;
#1646 = FACE_OUTER_BOUND ( 'NONE', #13158, .T. ) ;
#1647 = ORIENTED_EDGE ( 'NONE', *, *, #13509, .F. ) ;
#1648 = CARTESIAN_POINT ( 'NONE',  ( -2.828427124746189403, 2.828427124746190291, 16.00000000273119838 ) ) ;
#1649 = CARTESIAN_POINT ( 'NONE',  ( -19.99999999999999645, -9.000000000000003553, 10.00000000000008882 ) ) ;
#1650 = CARTESIAN_POINT ( 'NONE',  ( 52.46643183416157541, 7.028187705514638672, 13.68930817193508531 ) ) ;
#1651 = LINE ( 'NONE', #6817, #13751 ) ;
#1652 = CARTESIAN_POINT ( 'NONE',  ( 67.70000000109246230, 7.933012699999995476, 14.14382582708705094 ) ) ;
#1653 = VECTOR ( 'NONE', #22932, 1000.000000000000000 ) ;
#1654 = FACE_OUTER_BOUND ( 'NONE', #10152, .T. ) ;
#1655 = ORIENTED_EDGE ( 'NONE', *, *, #14504, .T. ) ;
#1656 = DIRECTION ( 'NONE',  ( -0.000000000000000000, -0.000000000000000000, -1.000000000000000000 ) ) ;
#1657 = VECTOR ( 'NONE', #15828, 1000.000000000000114 ) ;
#1658 = CARTESIAN_POINT ( 'NONE',  ( 56.71875000000000711, 13.00000000000000533, 16.24264068711927322 ) ) ;
#1659 = CARTESIAN_POINT ( 'NONE',  ( 4.000000000000000888, -1.656854249492379694, 0.8625000027311868767 ) ) ;
#1660 = DIRECTION ( 'NONE',  ( 0.000000000000000000, 0.000000000000000000, -1.000000000000000000 ) ) ;
#1661 = ORIENTED_EDGE ( 'NONE', *, *, #3484, .T. ) ;
#1662 = FACE_OUTER_BOUND ( 'NONE', #23691, .T. ) ;
#1663 = CARTESIAN_POINT ( 'NONE',  ( -3.458734125000000326, 0.000000000000000000, -2.262499998634403653 ) ) ;
#1664 = DIRECTION ( 'NONE',  ( -0.000000000000000000, -0.000000000000000000, -1.000000000000000000 ) ) ;
#1665 = EDGE_CURVE ( 'NONE', #19814, #6753, #17778, .T. ) ;
#1666 = EDGE_LOOP ( 'NONE', ( #4660, #14496, #2456, #7359 ) ) ;
#1667 = CARTESIAN_POINT ( 'NONE',  ( 6.396109596766199168, -9.000000000000005329, 10.00000000000008882 ) ) ;
#1668 = VERTEX_POINT ( 'NONE', #8568 ) ;
#1669 = LINE ( 'NONE', #17740, #23238 ) ;
#1670 = VECTOR ( 'NONE', #16250, 1000.000000000000000 ) ;
#1671 = CARTESIAN_POINT ( 'NONE',  ( 1.971781867644420635E-15, -4.000000000000000000, 19.25000000000001066 ) ) ;
#1672 = PLANE ( 'NONE',  #19525 ) ;
#1673 = LINE ( 'NONE', #21900, #11101 ) ;
#1674 = DIRECTION ( 'NONE',  ( 1.000000000000000000, 7.703719777548943412E-32, 0.000000000000000000 ) ) ;
#1675 = ADVANCED_FACE ( 'NONE', ( #12532 ), #16223, .F. ) ;
#1676 = CARTESIAN_POINT ( 'NONE',  ( -66.24999999999998579, 7.499999999999995559, 16.03553390593273420 ) ) ;
#1677 = DIRECTION ( 'NONE',  ( 1.000000000000000000, 0.000000000000000000, 0.000000000000000000 ) ) ;
#1678 = FACE_OUTER_BOUND ( 'NONE', #863, .T. ) ;
#1679 = FACE_OUTER_BOUND ( 'NONE', #7171, .T. ) ;
#1680 = CARTESIAN_POINT ( 'NONE',  ( -1.656854249492381248, -3.999999999999999112, 3.487500000000002487 ) ) ;
#1681 = CARTESIAN_POINT ( 'NONE',  ( -4.000000000000000000, -1.656854249492383024, 0.3625000000000019873 ) ) ;
#1682 = DIRECTION ( 'NONE',  ( -1.000000000000000000, 0.000000000000000000, 1.224646799147353207E-16 ) ) ;
#1683 = CARTESIAN_POINT ( 'NONE',  ( 1.025207404391860050E-15, 3.458734125000000326, 16.18750000136560629 ) ) ;
#1684 = DIRECTION ( 'NONE',  ( -0.5000000000000051070, 0.000000000000000000, 0.8660254037844355990 ) ) ;
#1685 = ORIENTED_EDGE ( 'NONE', *, *, #1427, .T. ) ;
#1686 = CARTESIAN_POINT ( 'NONE',  ( -70.55000000109247082, 8.538419263543522320, 16.46158073645647235 ) ) ;
#1687 = EDGE_LOOP ( 'NONE', ( #9119, #10883, #469, #20663 ) ) ;
#1688 = CARTESIAN_POINT ( 'NONE',  ( 52.93518183416157541, 9.931948859054379852, 18.99999999999999289 ) ) ;
#1689 = CARTESIAN_POINT ( 'NONE',  ( -66.20000000109247651, 12.06698730000000275, 14.14382582708705094 ) ) ;
#1690 = DIRECTION ( 'NONE',  ( -1.000000000000000000, 1.232595164407830672E-32, 2.736911063134408342E-48 ) ) ;
#1691 = CARTESIAN_POINT ( 'NONE',  ( 72.50000000000000000, 9.999999999999998224, 14.99999999999999645 ) ) ;
#1692 = EDGE_LOOP ( 'NONE', ( #12643, #19226, #4435, #11190 ) ) ;
#1693 = ORIENTED_EDGE ( 'NONE', *, *, #4155, .F. ) ;
#1694 = CYLINDRICAL_SURFACE ( 'NONE', #12537, 2.649999999999999467 ) ;
#1695 = CARTESIAN_POINT ( 'NONE',  ( 58.87500000000000711, 7.878679656440349177, 12.87867965644035984 ) ) ;
#1696 = AXIS2_PLACEMENT_3D ( 'NONE', #20506, #3629, #16465 ) ;
#1697 = CARTESIAN_POINT ( 'NONE',  ( -70.60000000109246798, 7.933012699999995476, 15.85617417291294196 ) ) ;
#1698 = CIRCLE ( 'NONE', #22751, 8.749000000000002331 ) ;
#1699 = ADVANCED_FACE ( 'NONE', ( #3394 ), #12407, .F. ) ;
#1700 = CARTESIAN_POINT ( 'NONE',  ( -69.90000000109246514, 9.143825827087049163, 17.06698729999999742 ) ) ;
#1701 = CARTESIAN_POINT ( 'NONE',  ( 2.445694354108821411, 2.445694354108820523, 14.31250000136560452 ) ) ;
#1702 = CARTESIAN_POINT ( 'NONE',  ( 4.999999999999999112, 6.807171995660675101, -6.478011392632816445 ) ) ;
#1703 = CARTESIAN_POINT ( 'NONE',  ( 53.71875000000002132, 13.00000000000000711, 16.24264068711927322 ) ) ;
#1704 = DIRECTION ( 'NONE',  ( 1.000000000000000000, 0.000000000000000000, 0.000000000000000000 ) ) ;
#1705 = CARTESIAN_POINT ( 'NONE',  ( 52.78125000000000711, 8.757359312880703683, 11.99999999999999822 ) ) ;
#1706 = CARTESIAN_POINT ( 'NONE',  ( -1.506022603841296270, 0.000000000000000000, 0.000000000000000000 ) ) ;
#1707 = ADVANCED_FACE ( 'NONE', ( #23509 ), #21828, .F. ) ;
#1708 = CARTESIAN_POINT ( 'NONE',  ( 1.411581201560190495E-15, 4.862606272033091592, -3.745885042887436622 ) ) ;
#1709 = ORIENTED_EDGE ( 'NONE', *, *, #11460, .T. ) ;
#1710 = CARTESIAN_POINT ( 'NONE',  ( 43.27628836966725601, -11.25000000000000355, 5.000000000000079936 ) ) ;
#1711 = FACE_OUTER_BOUND ( 'NONE', #15669, .T. ) ;
#1712 = VERTEX_POINT ( 'NONE', #6762 ) ;
#1713 = CARTESIAN_POINT ( 'NONE',  ( 53.53125000000000000, 11.24264068711929276, 18.00000000000000355 ) ) ;
#1714 = VECTOR ( 'NONE', #1604, 1000.000000000000000 ) ;
#1715 = FILL_AREA_STYLE_COLOUR ( '', #12211 ) ;
#1716 = CARTESIAN_POINT ( 'NONE',  ( 2.445694354108820079, 2.445694354108820523, 5.362500001365596347 ) ) ;
#1717 = VECTOR ( 'NONE', #16961, 999.9999999999997726 ) ;
#1718 = LINE ( 'NONE', #14330, #19683 ) ;
#1719 = VERTEX_POINT ( 'NONE', #8685 ) ;
#1720 = CARTESIAN_POINT ( 'NONE',  ( 2.828427124746192067, -2.828427124746189847, 18.37500000000001066 ) ) ;
#1721 = ORIENTED_EDGE ( 'NONE', *, *, #639, .F. ) ;
#1722 = CARTESIAN_POINT ( 'NONE',  ( -54.99999999999992895, 15.00000000000000000, 5.000000000000015987 ) ) ;
#1723 = CARTESIAN_POINT ( 'NONE',  ( 4.211140560182196957, 2.431303136016536470, -3.745885042887433514 ) ) ;
#1724 = ORIENTED_EDGE ( 'NONE', *, *, #5716, .F. ) ;
#1725 = PLANE ( 'NONE',  #11097 ) ;
#1726 = CARTESIAN_POINT ( 'NONE',  ( 55.00000000000000711, 15.00000000000000000, 10.00000000000000000 ) ) ;
#1727 =( BOUNDED_CURVE ( )  B_SPLINE_CURVE ( 2, ( #11098, #21719, #18143, #5334, #22191, #5563, #3416, #5680, #12676 ),
 .UNSPECIFIED., .F., .F. ) 
 B_SPLINE_CURVE_WITH_KNOTS ( ( 3, 2, 2, 2, 3 ),
 ( 0.8000000000000000444, 0.8125000000000000000, 0.8249999999999999556, 0.8375000000000000222, 0.8499999999999999778 ),
 .UNSPECIFIED. ) 
 CURVE ( )  GEOMETRIC_REPRESENTATION_ITEM ( )  RATIONAL_B_SPLINE_CURVE ( ( 1.000000000000000000, 0.9238795325112867385, 1.000000000000000000, 0.9238795325112867385, 1.000000000000000000, 0.9238795325112867385, 1.000000000000000000, 0.9238795325112867385, 1.000000000000000000 ) ) 
 REPRESENTATION_ITEM ( '' )  );
#1728 = ORIENTED_EDGE ( 'NONE', *, *, #10558, .T. ) ;
#1729 = CARTESIAN_POINT ( 'NONE',  ( 65.70000000109249072, 9.143825827087049163, 17.06698729999999742 ) ) ;
#1730 = EDGE_CURVE ( 'NONE', #18272, #11666, #15988, .T. ) ;
#1731 = CONICAL_SURFACE ( 'NONE', #12098, 2.500000000000000888, 0.9599310885968785900 ) ;
#1732 = CARTESIAN_POINT ( 'NONE',  ( 70.45000000000000284, 8.964466094067258695, 12.49999999999999289 ) ) ;
#1733 = ADVANCED_FACE ( 'NONE', ( #19672 ), #4509, .T. ) ;
#1734 = VECTOR ( 'NONE', #538, 1000.000000000000000 ) ;
#1735 = CARTESIAN_POINT ( 'NONE',  ( -1.301042606982605321E-15, 7.505553499465137612, -3.119443416399232394 ) ) ;
#1736 = CARTESIAN_POINT ( 'NONE',  ( 46.41788101966725577, -11.25000000000000355, 5.000000000000079936 ) ) ;
#1737 = CARTESIAN_POINT ( 'NONE',  ( 55.34606816583843880, 8.411196891453267099, 19.02818770551464667 ) ) ;
#1738 = CARTESIAN_POINT ( 'NONE',  ( -1.432654583217640276, 3.458734125000000326, -1.449999998634403653 ) ) ;
#1739 = EDGE_CURVE ( 'NONE', #7101, #5362, #20376, .T. ) ;
#1740 = SURFACE_STYLE_USAGE ( .BOTH. , #14468 ) ;
#1741 = FACE_OUTER_BOUND ( 'NONE', #8414, .T. ) ;
#1742 = CIRCLE ( 'NONE', #21616, 11.00000000000000000 ) ;
#1743 = EDGE_CURVE ( 'NONE', #10566, #4081, #12876, .T. ) ;
#1744 = AXIS2_PLACEMENT_3D ( 'NONE', #13997, #21258, #23435 ) ;
#1745 = DIRECTION ( 'NONE',  ( -0.9396926207859107594, -0.3420201433256623291, 1.540743955509804830E-32 ) ) ;
#1746 = VERTEX_POINT ( 'NONE', #3982 ) ;
#1747 = DIRECTION ( 'NONE',  ( 0.000000000000000000, 0.000000000000000000, 1.000000000000000000 ) ) ;
#1748 = CARTESIAN_POINT ( 'NONE',  ( 65.00000000000000000, -10.00000000000000178, 12.49999999999999467 ) ) ;
#1749 = CARTESIAN_POINT ( 'NONE',  ( 34.99999999999999289, 4.500000000000001776, -50.00000000000000000 ) ) ;
#1750 = ORIENTED_EDGE ( 'NONE', *, *, #9693, .F. ) ;
#1751 = ORIENTED_EDGE ( 'NONE', *, *, #3095, .T. ) ;
#1752 = FACE_OUTER_BOUND ( 'NONE', #14993, .T. ) ;
#1753 = CARTESIAN_POINT ( 'NONE',  ( 55.87500000000000711, 7.171572875253794166, 12.17157287525381726 ) ) ;
#1754 = ORIENTED_EDGE ( 'NONE', *, *, #4128, .F. ) ;
#1755 = CARTESIAN_POINT ( 'NONE',  ( -6.500000000000001776, -3.142418015001832821, -0.4043611937012249746 ) ) ;
#1756 = ORIENTED_EDGE ( 'NONE', *, *, #3903, .T. ) ;
#1757 = CARTESIAN_POINT ( 'NONE',  ( 54.65625000000001421, 6.000000000000004441, 16.65685424949239390 ) ) ;
#1758 = CARTESIAN_POINT ( 'NONE',  ( 69.15000000218495302, 12.50000000000000000, 13.96446609406725869 ) ) ;
#1759 = LINE ( 'NONE', #21873, #20990 ) ;
#1760 = CARTESIAN_POINT ( 'NONE',  ( 0.000000000000000000, -5.538577986808850717, -6.772677083992447500 ) ) ;
#1761 = ADVANCED_FACE ( 'NONE', ( #5907 ), #2582, .T. ) ;
#1762 = LINE ( 'NONE', #19728, #17185 ) ;
#1763 = EDGE_LOOP ( 'NONE', ( #23490, #23359, #7432, #18985 ) ) ;
#1764 = CARTESIAN_POINT ( 'NONE',  ( -2.828427124746188515, -2.828427124746190735, 17.25000000273119838 ) ) ;
#1765 = CARTESIAN_POINT ( 'NONE',  ( -19.99999999999999645, -9.000000000000003553, 5.000000000000079936 ) ) ;
#1766 = CARTESIAN_POINT ( 'NONE',  ( 57.81018183416157541, 14.00000000000000000, 15.06805114094561304 ) ) ;
#1767 = DIRECTION ( 'NONE',  ( 1.224646799147353207E-16, -0.000000000000000000, 1.000000000000000000 ) ) ;
#1768 = DIRECTION ( 'NONE',  ( 7.200064461366508930E-32, 1.000000000000000000, 5.754033390038004481E-16 ) ) ;
#1769 = CARTESIAN_POINT ( 'NONE',  ( 72.29999999999998295, 12.50000000000000000, 14.99999999999999645 ) ) ;
#1770 = EDGE_CURVE ( 'NONE', #13418, #16438, #7330, .T. ) ;
#1771 = CARTESIAN_POINT ( 'NONE',  ( 4.000000000000000000, 0.8378280264232961239, -3.220590601395640018 ) ) ;
#1772 = ORIENTED_EDGE ( 'NONE', *, *, #18829, .F. ) ;
#1773 = CYLINDRICAL_SURFACE ( 'NONE', #14305, 2.500000000000002220 ) ;
#1774 = CARTESIAN_POINT ( 'NONE',  ( 56.53125000000000711, 11.24264068711929276, 18.00000000000000000 ) ) ;
#1775 = FACE_OUTER_BOUND ( 'NONE', #22420, .T. ) ;
#1776 = ORIENTED_EDGE ( 'NONE', *, *, #5722, .F. ) ;
#1777 = CARTESIAN_POINT ( 'NONE',  ( -19.99999999999999645, -9.000000000000003553, 5.000000000000079936 ) ) ;
#1778 = CARTESIAN_POINT ( 'NONE',  ( 0.2500000000000002220, 0.000000000000000000, 4.000000000000000000 ) ) ;
#1779 = DIRECTION ( 'NONE',  ( 1.000000000000000000, 0.000000000000000000, 0.000000000000000000 ) ) ;
#1780 = ORIENTED_EDGE ( 'NONE', *, *, #23533, .F. ) ;
#1781 = DIRECTION ( 'NONE',  ( 0.000000000000000000, 0.000000000000000000, 1.000000000000000000 ) ) ;
#1782 = ORIENTED_EDGE ( 'NONE', *, *, #14781, .T. ) ;
#1783 = ORIENTED_EDGE ( 'NONE', *, *, #5073, .T. ) ;
#1784 = CARTESIAN_POINT ( 'NONE',  ( -3.999999999999999112, 0.000000000000000000, 21.31370849898476649 ) ) ;
#1785 = CARTESIAN_POINT ( 'NONE',  ( -2.828427124746188515, -2.828427124746190735, 18.12500000000001066 ) ) ;
#1786 = CARTESIAN_POINT ( 'NONE',  ( 45.00000000000000000, -7.098169556225942145, 56.71010071662853136 ) ) ;
#1787 = FACE_OUTER_BOUND ( 'NONE', #15021, .T. ) ;
#1788 = PRESENTATION_STYLE_ASSIGNMENT (( #5277 ) ) ;
#1789 = CARTESIAN_POINT ( 'NONE',  ( -4.898587196589412829E-16, 0.000000000000000000, -4.000000000000000000 ) ) ;
#1790 = VECTOR ( 'NONE', #4055, 1000.000000000000000 ) ;
#1791 = AXIS2_PLACEMENT_3D ( 'NONE', #12896, #285, #12679 ) ;
#1792 = CARTESIAN_POINT ( 'NONE',  ( -68.39999999999999147, 11.76776695296636888, 16.76776695296636532 ) ) ;
#1793 = CARTESIAN_POINT ( 'NONE',  ( 4.000000000000000888, -1.656854249492379694, -0.1374999972688121241 ) ) ;
#1794 = EDGE_CURVE ( 'NONE', #13420, #6899, #7969, .T. ) ;
#1795 = CARTESIAN_POINT ( 'NONE',  ( 3.458734125000002102, -1.432654583217639610, 18.87500000136560274 ) ) ;
#1796 = CARTESIAN_POINT ( 'NONE',  ( -35.00000000000000000, 4.500000000000003553, 4.286263797015736496E-15 ) ) ;
#1797 = CARTESIAN_POINT ( 'NONE',  ( 7.347880794884118750E-16, -4.000000000000000000, 4.549999999999999822 ) ) ;
#1798 = CARTESIAN_POINT ( 'NONE',  ( -0.3649867057748643617, 3.983313282257324950, 10.00000000000000888 ) ) ;
#1799 = CARTESIAN_POINT ( 'NONE',  ( 1.872352939448454495E-15, -3.458734125000000326, 12.68750000136560629 ) ) ;
#1800 = LINE ( 'NONE', #19650, #21017 ) ;
#1801 = APPLICATION_CONTEXT ( 'automotive_design' ) ;
#1802 = ORIENTED_EDGE ( 'NONE', *, *, #20831, .F. ) ;
#1803 = VECTOR ( 'NONE', #8957, 1000.000000000000000 ) ;
#1804 = CARTESIAN_POINT ( 'NONE',  ( -69.70000000109247651, 9.143825827087049163, 17.06698730000000097 ) ) ;
#1805 = EDGE_LOOP ( 'NONE', ( #18352, #23211, #22697, #21151 ) ) ;
#1806 = CARTESIAN_POINT ( 'NONE',  ( 53.21643183416158251, 13.97181229448536399, 16.72490539043799629 ) ) ;
#1807 = CARTESIAN_POINT ( 'NONE',  ( -68.90000000109247935, 9.143825827087049163, 17.06698729999999742 ) ) ;
#1808 = DIRECTION ( 'NONE',  ( 1.000000000000000000, 0.000000000000000000, 0.000000000000000000 ) ) ;
#1809 = CARTESIAN_POINT ( 'NONE',  ( 1.656854249492384135, -3.999999999999999112, 17.31250000000001066 ) ) ;
#1810 = ORIENTED_EDGE ( 'NONE', *, *, #2201, .F. ) ;
#1811 = VECTOR ( 'NONE', #23079, 1000.000000000000000 ) ;
#1812 = ORIENTED_EDGE ( 'NONE', *, *, #19152, .F. ) ;
#1813 = DIRECTION ( 'NONE',  ( 0.000000000000000000, 0.000000000000000000, -1.000000000000000000 ) ) ;
#1814 = CARTESIAN_POINT ( 'NONE',  ( 51.97106816583844591, 6.971812294485350670, 13.82541045382635403 ) ) ;
#1815 = CARTESIAN_POINT ( 'NONE',  ( -69.40000000109249356, 12.06698730000000275, 14.14382582708705094 ) ) ;
#1816 = CIRCLE ( 'NONE', #2585, 4.000000000000001776 ) ;
#1817 = CARTESIAN_POINT ( 'NONE',  ( -70.15000000109246514, 8.538419263543524096, 13.53841926354352054 ) ) ;
#1818 = CARTESIAN_POINT ( 'NONE',  ( 1.872352939448454495E-15, -3.458734125000000770, 10.93750000136560452 ) ) ;
#1819 = CARTESIAN_POINT ( 'NONE',  ( 1.656854249492384135, -3.999999999999999112, 10.43750000273119660 ) ) ;
#1820 = CARTESIAN_POINT ( 'NONE',  ( 55.12500000000000711, 12.12132034355964727, 17.12132034355963484 ) ) ;
#1821 = CARTESIAN_POINT ( 'NONE',  ( 71.89999999999999147, 7.499999999999996447, 14.99999999999999645 ) ) ;
#1822 = AXIS2_PLACEMENT_3D ( 'NONE', #20393, #873, #8206 ) ;
#1823 = VECTOR ( 'NONE', #6635, 1000.000000000000114 ) ;
#1824 = CARTESIAN_POINT ( 'NONE',  ( 53.71875000000002132, 13.00000000000000711, 16.24264068711927322 ) ) ;
#1825 = FACE_OUTER_BOUND ( 'NONE', #22054, .T. ) ;
#1826 = LINE ( 'NONE', #21939, #17225 ) ;
#1827 = ORIENTED_EDGE ( 'NONE', *, *, #23114, .T. ) ;
#1828 = FACE_OUTER_BOUND ( 'NONE', #2269, .T. ) ;
#1829 = CARTESIAN_POINT ( 'NONE',  ( -70.14999999999999147, 8.964466094067256918, 17.49999999999999289 ) ) ;
#1830 = EDGE_LOOP ( 'NONE', ( #514, #19043, #17039, #9791 ) ) ;
#1831 = CARTESIAN_POINT ( 'NONE',  ( 51.93750000000000711, 10.00000000000000711, 17.99999999999999645 ) ) ;
#1832 = SURFACE_STYLE_FILL_AREA ( #12668 ) ;
#1833 = CARTESIAN_POINT ( 'NONE',  ( -1.432654583217640276, 3.458734125000000326, 4.550000001365596347 ) ) ;
#1834 = LINE ( 'NONE', #9184, #13242 ) ;
#1835 = VERTEX_POINT ( 'NONE', #7480 ) ;
#1836 = CARTESIAN_POINT ( 'NONE',  ( -3.999999999999999112, 0.000000000000000000, 16.00000000000001066 ) ) ;
#1837 = EDGE_CURVE ( 'NONE', #17270, #14716, #4102, .T. ) ;
#1838 = CARTESIAN_POINT ( 'NONE',  ( -2.100000000000000089, 2.571758278209441957E-16, -5.000000000000000000 ) ) ;
#1839 = CARTESIAN_POINT ( 'NONE',  ( 27.56832511966726784, -11.25000000000000355, 5.000000000000079936 ) ) ;
#1840 = ORIENTED_EDGE ( 'NONE', *, *, #8806, .F. ) ;
#1841 = FACE_OUTER_BOUND ( 'NONE', #21249, .T. ) ;
#1842 = AXIS2_PLACEMENT_3D ( 'NONE', #14714, #21971, #12911 ) ;
#1843 = CARTESIAN_POINT ( 'NONE',  ( 45.00000000000000000, -14.69846310392956745, 35.82846581308617573 ) ) ;
#1844 = EDGE_CURVE ( 'NONE', #13106, #19458, #9139, .T. ) ;
#1845 = CARTESIAN_POINT ( 'NONE',  ( 2.445694354108820967, -2.445694354108820079, 0.3625000013655968467 ) ) ;
#1846 = CARTESIAN_POINT ( 'NONE',  ( 67.79999999999999716, 8.232233047033627571, 16.76776695296636532 ) ) ;
#1847 = CIRCLE ( 'NONE', #13414, 4.250000000000000000 ) ;
#1848 = FACE_OUTER_BOUND ( 'NONE', #12091, .T. ) ;
#1849 = CIRCLE ( 'NONE', #20210, 8.265000000000021885 ) ;
#1850 = CARTESIAN_POINT ( 'NONE',  ( -54.99999999999992895, 15.00000000000000000, 5.000000000000015987 ) ) ;
#1851 = CARTESIAN_POINT ( 'NONE',  ( 51.31481816583844591, 14.00000000000000178, 14.93194885905434610 ) ) ;
#1852 = CARTESIAN_POINT ( 'NONE',  ( 3.458734125000000770, -1.432654583217639610, -1.824999998634404097 ) ) ;
#1853 = FACE_OUTER_BOUND ( 'NONE', #22121, .T. ) ;
#1854 = CYLINDRICAL_SURFACE ( 'NONE', #2105, 2.500000000000002220 ) ;
#1855 = DIRECTION ( 'NONE',  ( 0.000000000000000000, 0.000000000000000000, 1.000000000000000000 ) ) ;
#1856 = VERTEX_POINT ( 'NONE', #16932 ) ;
#1857 = DIRECTION ( 'NONE',  ( 0.000000000000000000, 0.000000000000000000, 1.000000000000000000 ) ) ;
#1858 = AXIS2_PLACEMENT_3D ( 'NONE', #14634, #16643, #5504 ) ;
#1859 = PLANE ( 'NONE',  #18241 ) ;
#1860 = DIRECTION ( 'NONE',  ( -0.000000000000000000, 0.000000000000000000, -1.000000000000000000 ) ) ;
#1861 = ORIENTED_EDGE ( 'NONE', *, *, #5688, .F. ) ;
#1862 = ORIENTED_EDGE ( 'NONE', *, *, #14206, .T. ) ;
#1863 = ADVANCED_FACE ( 'NONE', ( #22044 ), #4904, .T. ) ;
#1864 = CARTESIAN_POINT ( 'NONE',  ( 4.999999999999999112, 0.000000000000000000, 0.000000000000000000 ) ) ;
#1865 = ADVANCED_FACE ( 'NONE', ( #7723 ), #3867, .T. ) ;
#1866 = VECTOR ( 'NONE', #21905, 1000.000000000000000 ) ;
#1867 = CARTESIAN_POINT ( 'NONE',  ( 53.90625000000000000, 13.99999999999999289, 13.34314575050759544 ) ) ;
#1868 = ORIENTED_EDGE ( 'NONE', *, *, #342, .F. ) ;
#1869 = CARTESIAN_POINT ( 'NONE',  ( -6.500000000000000000, 0.000000000000000000, 1.734723475976807094E-15 ) ) ;
#1870 = ORIENTED_EDGE ( 'NONE', *, *, #19457, .F. ) ;
#1871 = VECTOR ( 'NONE', #9335, 1000.000000000000000 ) ;
#1872 = CARTESIAN_POINT ( 'NONE',  ( 56.09606816583844591, 11.58880310854672935, 10.97181229448534445 ) ) ;
#1873 = EDGE_CURVE ( 'NONE', #19365, #1924, #15036, .T. ) ;
#1874 = CARTESIAN_POINT ( 'NONE',  ( 71.60000000109246798, 9.143825827087050939, 12.93301269999999370 ) ) ;
#1875 = AXIS2_PLACEMENT_3D ( 'NONE', #10836, #1330, #5416 ) ;
#1876 = STYLED_ITEM ( 'NONE', ( #1013 ), #19027 ) ;
#1877 = CARTESIAN_POINT ( 'NONE',  ( -1.506022603841227436, 0.000000000000000000, 0.000000000000000000 ) ) ;
#1878 = CARTESIAN_POINT ( 'NONE',  ( 118.3095189484530181, 7.098169556225943033, 56.71010071662853136 ) ) ;
#1879 = DIRECTION ( 'NONE',  ( -1.000000000000000000, 0.000000000000000000, 9.637352644315595243E-17 ) ) ;
#1880 = ORIENTED_EDGE ( 'NONE', *, *, #23008, .T. ) ;
#1881 = CARTESIAN_POINT ( 'NONE',  ( -3.999999999999999112, 0.000000000000000000, 11.00000000000001066 ) ) ;
#1882 = CARTESIAN_POINT ( 'NONE',  ( 1.236993788156008760E-15, 0.000000000000000000, -20.00000000000000000 ) ) ;
#1883 = ADVANCED_BREP_SHAPE_REPRESENTATION ( '', ( #6242, #7318 ), #5664 ) ;
#1884 = CARTESIAN_POINT ( 'NONE',  ( 55.27893183416158251, 8.411196891453236901, 10.97181229448535511 ) ) ;
#1885 = CARTESIAN_POINT ( 'NONE',  ( 72.50000000000000000, 9.999999999999998224, 14.99999999999999645 ) ) ;
#1886 = AXIS2_PLACEMENT_3D ( 'NONE', #16187, #10818, #12617 ) ;
#1887 = CARTESIAN_POINT ( 'NONE',  ( 32.13446180928345086, -8.974600000000002353, 5.000000000000079936 ) ) ;
#1888 = CARTESIAN_POINT ( 'NONE',  ( -67.74999999999997158, 8.964466094067246260, 17.49999999999999289 ) ) ;
#1889 = AXIS2_PLACEMENT_3D ( 'NONE', #22318, #533, #7508 ) ;
#1890 = CARTESIAN_POINT ( 'NONE',  ( 4.211405965630455661, 2.460463115436283932, -3.751298928144577882 ) ) ;
#1891 = ORIENTED_EDGE ( 'NONE', *, *, #13776, .T. ) ;
#1892 = LINE ( 'NONE', #7320, #4724 ) ;
#1893 = CARTESIAN_POINT ( 'NONE',  ( 51.09375000000000711, 11.24264068711927322, 11.99999999999998934 ) ) ;
#1894 = EDGE_CURVE ( 'NONE', #18318, #20532, #21936, .T. ) ;
#1895 = FACE_OUTER_BOUND ( 'NONE', #10910, .T. ) ;
#1896 = ORIENTED_EDGE ( 'NONE', *, *, #15551, .T. ) ;
#1897 = CARTESIAN_POINT ( 'NONE',  ( 4.999999999999999112, -4.762163868918204201, -9.915734732513268312 ) ) ;
#1898 = CARTESIAN_POINT ( 'NONE',  ( -3.458734125000000326, 1.432654583217640276, -3.324999998634403209 ) ) ;
#1899 = CARTESIAN_POINT ( 'NONE',  ( 3.510273485745307731, 2.827716139362654424, -3.610536846335885564 ) ) ;
#1900 = CIRCLE ( 'NONE', #14558, 4.000000000000000000 ) ;
#1901 = EDGE_CURVE ( 'NONE', #11881, #10070, #12778, .T. ) ;
#1902 = ORIENTED_EDGE ( 'NONE', *, *, #11855, .T. ) ;
#1903 = CARTESIAN_POINT ( 'NONE',  ( 4.000000000000000000, -1.084202172485504434E-14, -3.142992957459231906 ) ) ;
#1904 = VERTEX_POINT ( 'NONE', #260 ) ;
#1905 = LINE ( 'NONE', #22251, #16017 ) ;
#1906 = CARTESIAN_POINT ( 'NONE',  ( 2.828427124746192067, -2.828427124746189847, 19.37500000000001066 ) ) ;
#1907 = EDGE_CURVE ( 'NONE', #7079, #2314, #16812, .T. ) ;
#1908 = CARTESIAN_POINT ( 'NONE',  ( 2.500000000000000000, -1.178949249685214307, 2.042000000000001592 ) ) ;
#1909 = CIRCLE ( 'NONE', #4587, 2.500000000000007550 ) ;
#1910 = EDGE_CURVE ( 'NONE', #19081, #21422, #12084, .T. ) ;
#1911 = CYLINDRICAL_SURFACE ( 'NONE', #355, 2.649999999999992806 ) ;
#1912 = FILL_AREA_STYLE_COLOUR ( '', #12584 ) ;
#1913 = VERTEX_POINT ( 'NONE', #16458 ) ;
#1914 = AXIS2_PLACEMENT_3D ( 'NONE', #17590, #19709, #1154 ) ;
#1915 = CARTESIAN_POINT ( 'NONE',  ( -67.25000000000000000, 8.964466094067258695, 12.49999999999999289 ) ) ;
#1916 = CARTESIAN_POINT ( 'NONE',  ( 4.714285714285714413, 0.000000000000000000, 9.480888224575631185 ) ) ;
#1917 = CARTESIAN_POINT ( 'NONE',  ( 66.45000000109247651, 9.999999999999998224, 17.06698730000000097 ) ) ;
#1918 = CARTESIAN_POINT ( 'NONE',  ( 3.458734125000001214, 4.235727675282971730E-16, 15.93750000136560629 ) ) ;
#1919 = DIRECTION ( 'NONE',  ( -1.000000000000000000, 0.000000000000000000, 1.445602896647339163E-16 ) ) ;
#1920 = CARTESIAN_POINT ( 'NONE',  ( -2.449293598294706907E-16, 4.000000000000000000, 6.050000000000001599 ) ) ;
#1921 = FACE_OUTER_BOUND ( 'NONE', #4705, .T. ) ;
#1922 = CARTESIAN_POINT ( 'NONE',  ( -2.445694354108818303, -2.445694354108820523, 12.56250000136560629 ) ) ;
#1923 = CARTESIAN_POINT ( 'NONE',  ( 2.500000000000000000, 1.178949249685212974, -2.042000000000001148 ) ) ;
#1924 = VERTEX_POINT ( 'NONE', #392 ) ;
#1925 = CARTESIAN_POINT ( 'NONE',  ( -67.70000000109247651, 10.85617417291294551, 12.93301269999999192 ) ) ;
#1926 = ORIENTED_EDGE ( 'NONE', *, *, #9858, .T. ) ;
#1927 = CARTESIAN_POINT ( 'NONE',  ( 58.27893183416158962, 8.411196891453236901, 10.97181229448535511 ) ) ;
#1928 = CARTESIAN_POINT ( 'NONE',  ( -71.25000000109247367, 12.06698730000000097, 14.99999999999999645 ) ) ;
#1929 = PRODUCT_CONTEXT ( 'NONE', #12856, 'mechanical' ) ;
#1930 = DIRECTION ( 'NONE',  ( -1.224646799147353207E-16, 0.000000000000000000, -1.000000000000000000 ) ) ;
#1931 = VERTEX_POINT ( 'NONE', #20962 ) ;
#1932 = VECTOR ( 'NONE', #20953, 1000.000000000000000 ) ;
#1933 = ORIENTED_EDGE ( 'NONE', *, *, #10842, .F. ) ;
#1934 = CARTESIAN_POINT ( 'NONE',  ( -3.458734124999999437, 0.000000000000000000, 19.68750000136560629 ) ) ;
#1935 = ADVANCED_FACE ( 'NONE', ( #15270 ), #2532, .F. ) ;
#1936 = CARTESIAN_POINT ( 'NONE',  ( 52.25231816583844591, 7.926799079670502124, 17.16943976678978245 ) ) ;
#1937 = EDGE_CURVE ( 'NONE', #21119, #4764, #20733, .T. ) ;
#1938 = CARTESIAN_POINT ( 'NONE',  ( -70.95000000109247651, 11.46158073645647235, 13.53841926354352232 ) ) ;
#1939 = SHAPE_REPRESENTATION ( 'torque nut 08a_iso_ISO 10511-M8-N', ( #7318 ), #9900 ) ;
#1940 = CARTESIAN_POINT ( 'NONE',  ( -69.00000000109245946, 10.85617417291294551, 17.06698729999999742 ) ) ;
#1941 = CARTESIAN_POINT ( 'NONE',  ( -2.445694354108819191, 2.445694354108820523, 12.56250000136560629 ) ) ;
#1942 = CARTESIAN_POINT ( 'NONE',  ( 13.29415075323381323, -9.000000000000001776, 5.000000000000079936 ) ) ;
#1943 = CARTESIAN_POINT ( 'NONE',  ( 54.28125000000000000, 8.757359312880703683, 11.99999999999999822 ) ) ;
#1944 = AXIS2_PLACEMENT_3D ( 'NONE', #8248, #20792, #13523 ) ;
#1945 = CARTESIAN_POINT ( 'NONE',  ( 4.999999999999999112, -2.223716399045630343, 8.461683424509308438 ) ) ;
#1946 = CARTESIAN_POINT ( 'NONE',  ( 54.75000000000000711, 7.878679656440361612, 17.12132034355964549 ) ) ;
#1947 = CARTESIAN_POINT ( 'NONE',  ( -3.999999999999999112, 1.656854249492380804, 16.06250000273119838 ) ) ;
#1948 = CARTESIAN_POINT ( 'NONE',  ( 50.00000000000000000, -2.399706452296352932, 60.00000000000021316 ) ) ;
#1949 = VERTEX_POINT ( 'NONE', #22892 ) ;
#1950 = CYLINDRICAL_SURFACE ( 'NONE', #8702, 8.265000000000021885 ) ;
#1951 = CARTESIAN_POINT ( 'NONE',  ( -0.5636800770129166693, -4.293361309317430319, -3.531542292955206275 ) ) ;
#1952 = ORIENTED_EDGE ( 'NONE', *, *, #11567, .F. ) ;
#1953 = CARTESIAN_POINT ( 'NONE',  ( 52.31250000000000711, 13.00000000000000000, 14.99999999999998757 ) ) ;
#1954 = CARTESIAN_POINT ( 'NONE',  ( 2.445694354108820079, 2.445694354108820523, 4.362500001365595459 ) ) ;
#1955 = CARTESIAN_POINT ( 'NONE',  ( 4.000000000000000000, 4.898587196589412829E-16, 1.800000000000001155 ) ) ;
#1956 = ORIENTED_EDGE ( 'NONE', *, *, #18593, .T. ) ;
#1957 = B_SPLINE_CURVE_WITH_KNOTS ( 'NONE', 3,
 ( #11259, #5735, #13064, #5846, #7780, #11378, #20319, #331 ),
 .UNSPECIFIED., .F., .F.,
 ( 4, 2, 2, 4 ),
 ( 0.003797433802554438069, 0.004743183970586236156, 0.005688934138618034243, 0.007580434474681629550 ),
 .UNSPECIFIED. ) ;
#1958 = CARTESIAN_POINT ( 'NONE',  ( 2.828427124746192067, -2.828427124746189847, 16.37500000000001066 ) ) ;
#1959 = LINE ( 'NONE', #5447, #11042 ) ;
#1960 = ORIENTED_EDGE ( 'NONE', *, *, #1992, .T. ) ;
#1961 = CARTESIAN_POINT ( 'NONE',  ( -4.898587196589412829E-16, 0.000000000000000000, -4.000000000000000000 ) ) ;
#1962 = CARTESIAN_POINT ( 'NONE',  ( 20.00000000000000355, 4.500000000000003553, -2.449293598294706907E-15 ) ) ;
#1963 = CARTESIAN_POINT ( 'NONE',  ( 6.353591512924457348E-16, -3.458734125000000770, 0.2375000013655967357 ) ) ;
#1964 = CARTESIAN_POINT ( 'NONE',  ( 69.70000000000000284, 9.999999999999998224, 12.49999999999999289 ) ) ;
#1965 = CARTESIAN_POINT ( 'NONE',  ( 4.999999999999999112, 4.057423117305515525, -8.475820894092930047 ) ) ;
#1966 = EDGE_CURVE ( 'NONE', #6314, #9649, #2882, .T. ) ;
#1967 = CARTESIAN_POINT ( 'NONE',  ( -27.50000000000000711, 1.500000000000003109, -31.01025403784446510 ) ) ;
#1968 = CARTESIAN_POINT ( 'NONE',  ( 51.22106816583844591, 14.02818770551465377, 16.58880310854672757 ) ) ;
#1969 = CARTESIAN_POINT ( 'NONE',  ( 2.445694354108820523, -2.445694354108820079, -0.8874999986344025427 ) ) ;
#1970 = CARTESIAN_POINT ( 'NONE',  ( -3.458734124999999437, 1.432654583217640498, 15.62500000136560629 ) ) ;
#1971 = DIRECTION ( 'NONE',  ( 0.000000000000000000, 0.000000000000000000, -1.000000000000000000 ) ) ;
#1972 = DIRECTION ( 'NONE',  ( 1.000000000000000000, 0.000000000000000000, 0.000000000000000000 ) ) ;
#1973 = CARTESIAN_POINT ( 'NONE',  ( 0.000000000000000000, 10.90201369670498721, 1.464956435139581403 ) ) ;
#1974 = VERTEX_POINT ( 'NONE', #2419 ) ;
#1975 = CARTESIAN_POINT ( 'NONE',  ( -3.999999999999999112, 0.000000000000000000, 12.12500000273119838 ) ) ;
#1976 = CARTESIAN_POINT ( 'NONE',  ( -2.688821387764050996E-14, -4.618802153517012954, -0.4999999999999995559 ) ) ;
#1977 = LINE ( 'NONE', #5353, #6317 ) ;
#1978 = VERTEX_POINT ( 'NONE', #17404 ) ;
#1979 = EDGE_LOOP ( 'NONE', ( #21980, #9928, #1104, #8440 ) ) ;
#1980 = DIRECTION ( 'NONE',  ( 0.000000000000000000, 0.000000000000000000, 1.000000000000000000 ) ) ;
#1981 = VERTEX_POINT ( 'NONE', #13582 ) ;
#1982 = CARTESIAN_POINT ( 'NONE',  ( 59.06250000000000711, 5.999999999999996447, 15.00000000000001599 ) ) ;
#1983 = EDGE_LOOP ( 'NONE', ( #13921, #10487, #4144, #18954 ) ) ;
#1984 = DIRECTION ( 'NONE',  ( 0.000000000000000000, 0.9510565162951521989, 0.3090169943749515591 ) ) ;
#1985 = ORIENTED_EDGE ( 'NONE', *, *, #13640, .F. ) ;
#1986 = CARTESIAN_POINT ( 'NONE',  ( 55.43981816583843170, 10.06805114094564857, 19.00000000000000000 ) ) ;
#1987 = AXIS2_PLACEMENT_3D ( 'NONE', #4169, #22358, #10062 ) ;
#1988 = CARTESIAN_POINT ( 'NONE',  ( 70.65000000109247935, 7.933012699999995476, 14.99999999999999645 ) ) ;
#1989 = LINE ( 'NONE', #20550, #20553 ) ;
#1990 = EDGE_LOOP ( 'NONE', ( #6524, #5819, #17095, #15250 ) ) ;
#1991 = CARTESIAN_POINT ( 'NONE',  ( -3.999999999999999112, 1.656854249492380804, 10.93750000000001421 ) ) ;
#1992 = EDGE_CURVE ( 'NONE', #19485, #11205, #3180, .T. ) ;
#1993 = CARTESIAN_POINT ( 'NONE',  ( -3.028668353233801458, -9.000000000000005329, 5.000000000000079936 ) ) ;
#1994 = EDGE_CURVE ( 'NONE', #19611, #2045, #6256, .T. ) ;
#1995 = CARTESIAN_POINT ( 'NONE',  ( 59.15625000000002132, 6.000000000000004441, 16.65685424949239390 ) ) ;
#1996 = DIRECTION ( 'NONE',  ( 0.000000000000000000, 0.000000000000000000, -1.000000000000000000 ) ) ;
#1997 = DIRECTION ( 'NONE',  ( 0.000000000000000000, 0.000000000000000000, 1.000000000000000000 ) ) ;
#1998 = DIRECTION ( 'NONE',  ( 0.000000000000000000, 0.000000000000000000, -1.000000000000000000 ) ) ;
#1999 = CARTESIAN_POINT ( 'NONE',  ( 4.000000000000000000, -1.677850389431204459, -3.535268758346977513 ) ) ;
#2000 = ORIENTED_EDGE ( 'NONE', *, *, #1770, .T. ) ;
#2001 = FACE_OUTER_BOUND ( 'NONE', #18168, .T. ) ;
#2002 = CARTESIAN_POINT ( 'NONE',  ( 52.31250000000000711, 13.00000000000000000, 14.99999999999998757 ) ) ;
#2003 = DIRECTION ( 'NONE',  ( -1.000000000000000000, 0.000000000000000000, 0.000000000000000000 ) ) ;
#2004 = SURFACE_STYLE_FILL_AREA ( #5852 ) ;
#2005 = EDGE_CURVE ( 'NONE', #19770, #17091, #9326, .T. ) ;
#2006 = VERTEX_POINT ( 'NONE', #22655 ) ;
#2007 = CARTESIAN_POINT ( 'NONE',  ( -4.000000000000000888, -1.539600717839011201, -3.300726591567081591 ) ) ;
#2008 = CARTESIAN_POINT ( 'NONE',  ( 70.89999999999999147, 9.999999999999998224, 17.49999999999999645 ) ) ;
#2009 = CARTESIAN_POINT ( 'NONE',  ( 3.861362476283255685, 2.629030857715988656, -3.671615880910370500 ) ) ;
#2010 = CARTESIAN_POINT ( 'NONE',  ( -3.999999999999999112, 0.000000000000000000, 10.12500000273119660 ) ) ;
#2011 = ORIENTED_EDGE ( 'NONE', *, *, #18486, .F. ) ;
#2012 = LINE ( 'NONE', #16764, #18322 ) ;
#2013 = ORIENTED_EDGE ( 'NONE', *, *, #20277, .T. ) ;
#2014 = CARTESIAN_POINT ( 'NONE',  ( -1.656854249492379472, 4.000000000000000000, 18.93750000273119838 ) ) ;
#2015 = CARTESIAN_POINT ( 'NONE',  ( 4.000000000000000888, 4.898587196589412829E-16, 14.50000000000001066 ) ) ;
#2016 = CARTESIAN_POINT ( 'NONE',  ( -14.99999999999997335, -15.00000000000000000, -49.99999999999999289 ) ) ;
#2017 = DIRECTION ( 'NONE',  ( 0.000000000000000000, 0.000000000000000000, -1.000000000000000000 ) ) ;
#2018 = CARTESIAN_POINT ( 'NONE',  ( 0.000000000000000000, 0.000000000000000000, 0.000000000000000000 ) ) ;
#2019 = CARTESIAN_POINT ( 'NONE',  ( 70.50000000109247367, 12.06698729999999919, 15.85617417291294196 ) ) ;
#2020 = VERTEX_POINT ( 'NONE', #8302 ) ;
#2021 = VECTOR ( 'NONE', #22689, 1000.000000000000000 ) ;
#2022 = ADVANCED_FACE ( 'NONE', ( #21083, #15623 ), #856, .T. ) ;
#2023 = CARTESIAN_POINT ( 'NONE',  ( -60.00000000000000711, -15.00000000000000000, 10.00000000000004974 ) ) ;
#2024 = AXIS2_PLACEMENT_3D ( 'NONE', #6122, #13326, #7925 ) ;
#2025 = ADVANCED_FACE ( 'NONE', ( #10000 ), #6023, .T. ) ;
#2026 = DIRECTION ( 'NONE',  ( 1.000000000000000000, 0.000000000000000000, 0.000000000000000000 ) ) ;
#2027 = CARTESIAN_POINT ( 'NONE',  ( 71.70000000109247651, 7.933012699999995476, 14.14382582708705094 ) ) ;
#2028 = CARTESIAN_POINT ( 'NONE',  ( -2.445694354108819191, 2.445694354108820523, 16.31250000136560629 ) ) ;
#2029 = DIRECTION ( 'NONE',  ( 1.224646799147353207E-16, 0.000000000000000000, 1.000000000000000000 ) ) ;
#2030 = CARTESIAN_POINT ( 'NONE',  ( -2.445694354108819635, -2.445694354108820967, -2.887499998634404097 ) ) ;
#2031 = CARTESIAN_POINT ( 'NONE',  ( -2.449293598294706907E-16, 4.000000000000000000, 5.050000000000000711 ) ) ;
#2032 = CARTESIAN_POINT ( 'NONE',  ( 7.347880794884118750E-16, -4.000000000000000000, -3.324999997268812901 ) ) ;
#2033 = CARTESIAN_POINT ( 'NONE',  ( 2.445694354108821411, 2.445694354108820523, 12.06250000136560629 ) ) ;
#2034 = DIRECTION ( 'NONE',  ( 0.000000000000000000, 0.000000000000000000, 1.000000000000000000 ) ) ;
#2035 = ADVANCED_FACE ( 'NONE', ( #11563 ), #19293, .F. ) ;
#2036 = PRODUCT_DEFINITION_SHAPE ( 'NONE', 'NONE',  #23707 ) ;
#2037 = ADVANCED_FACE ( 'NONE', ( #13351 ), #19066, .T. ) ;
#2038 = EDGE_LOOP ( 'NONE', ( #7103, #10512, #10582, #2161 ) ) ;
#2039 = CARTESIAN_POINT ( 'NONE',  ( -68.05000000109247082, 9.999999999999998224, 17.06698730000000097 ) ) ;
#2040 = ORIENTED_EDGE ( 'NONE', *, *, #16782, .T. ) ;
#2041 = CARTESIAN_POINT ( 'NONE',  ( 54.15393183416158251, 5.971812294485358663, 16.58880310854675599 ) ) ;
#2042 = CARTESIAN_POINT ( 'NONE',  ( -69.60000000109248219, 12.06698730000000275, 14.14382582708705094 ) ) ;
#2043 = DIRECTION ( 'NONE',  ( 0.000000000000000000, 0.000000000000000000, 1.000000000000000000 ) ) ;
#2044 = VERTEX_POINT ( 'NONE', #6262 ) ;
#2045 = VERTEX_POINT ( 'NONE', #12029 ) ;
#2046 = CARTESIAN_POINT ( 'NONE',  ( 24.42673246966726452, -11.25000000000000355, 5.000000000000079936 ) ) ;
#2047 = CARTESIAN_POINT ( 'NONE',  ( 54.00000000000000711, 12.12132034355963484, 12.87867965644034740 ) ) ;
#2048 = CARTESIAN_POINT ( 'NONE',  ( -65.75000000218494733, 8.964466094067258695, 12.49999999999999289 ) ) ;
#2049 = CARTESIAN_POINT ( 'NONE',  ( -70.00000000109247367, 7.933012699999995476, 15.85617417291294196 ) ) ;
#2050 = CARTESIAN_POINT ( 'NONE',  ( -3.458734124999998105, -1.432654583217642497, 10.75000000136560452 ) ) ;
#2051 = EDGE_CURVE ( 'NONE', #12043, #8977, #6382, .T. ) ;
#2052 = PLANE ( 'NONE',  #11510 ) ;
#2053 = CARTESIAN_POINT ( 'NONE',  ( 55.68750000000000000, 9.999999999999989342, 11.99999999999999467 ) ) ;
#2054 = DIRECTION ( 'NONE',  ( 0.5000000000000022204, 0.8660254037844374864, -0.000000000000000000 ) ) ;
#2055 = EDGE_CURVE ( 'NONE', #23001, #2788, #13699, .T. ) ;
#2056 = CARTESIAN_POINT ( 'NONE',  ( 2.500000000000000000, 2.357898499370431722, -2.818925648462311528E-15 ) ) ;
#2057 = CARTESIAN_POINT ( 'NONE',  ( -3.458734124999998105, -1.432654583217642275, 12.50000000136560629 ) ) ;
#2058 = CARTESIAN_POINT ( 'NONE',  ( 4.000000000000000888, 4.898587196589412829E-16, 15.62500000273119660 ) ) ;
#2059 = AXIS2_PLACEMENT_3D ( 'NONE', #10357, #21086, #8435 ) ;
#2060 = DIRECTION ( 'NONE',  ( 0.000000000000000000, 0.000000000000000000, 1.000000000000000000 ) ) ;
#2061 = EDGE_CURVE ( 'NONE', #4680, #2595, #5100, .T. ) ;
#2062 = ORIENTED_EDGE ( 'NONE', *, *, #3302, .F. ) ;
#2063 = LINE ( 'NONE', #14684, #18233 ) ;
#2064 = CARTESIAN_POINT ( 'NONE',  ( -71.45000000218495018, 11.03553390593275374, 12.50000000000001243 ) ) ;
#2065 = ORIENTED_EDGE ( 'NONE', *, *, #4433, .T. ) ;
#2066 = CARTESIAN_POINT ( 'NONE',  ( 53.90625000000000000, 12.99999999999999645, 13.75735931288070191 ) ) ;
#2067 = CARTESIAN_POINT ( 'NONE',  ( -4.000000000000000888, 1.656854249492380804, -3.637499997268812013 ) ) ;
#2068 = VECTOR ( 'NONE', #4163, 1000.000000000000000 ) ;
#2069 = DIRECTION ( 'NONE',  ( 0.000000000000000000, 0.000000000000000000, 1.000000000000000000 ) ) ;
#2070 = ORIENTED_EDGE ( 'NONE', *, *, #7765, .F. ) ;
#2071 = CARTESIAN_POINT ( 'NONE',  ( 4.000000000000000888, 4.898587196589412829E-16, 13.50000000000001066 ) ) ;
#2072 = CARTESIAN_POINT ( 'NONE',  ( 1.489200000000000079, 1.009010990753487416E-15, 8.239200000000002078 ) ) ;
#2073 = VECTOR ( 'NONE', #10600, 1000.000000000000114 ) ;
#2074 =( BOUNDED_SURFACE ( )  B_SPLINE_SURFACE ( 1, 2, ( 
 ( #21337, #17774, #15764, #12528, #19790, #6530, #1345, #6645, #13849, #13959, #14198, #4833, #12164, #19434, #14559, #9279, #11197, #3862, #7242, #18589, #22170, #23505, #14671, #5658, #9391, #11073, #20256, #7119, #16564, #33, #12872, #9166, #9044, #3733, #14792, #16685, #14432, #22040, #3512, #21823, #10845, #2173, #1817, #12992, #16218, #2049, #21931, #1700, #5426, #21698, #12763, #7590, #18359, #13113, #18471, #7363, #16454, #20127, #16334, #5784, #23629, #5540, #256, #5308, #14911, #1940, #3617, #144, #10957, #12649, #7476, #20372, #3978, #11315, #19909, #20015, #18121, #18234, #15265, #5904, #16928, #7719, #6258, #13696, #2302, #4579, #853, #9996, #11914, #20959, #388, #22289, #18945, #17286, #19182, #9510, #20617, #13578, #506, #9868, #11792, #16807, #11439, #22769, #19063, #15032, #7828, #13229, #20494, #4098, #17163, #18713, #6147, #8077, #9747, #22410, #20846, #2654, #18830, #2416, #4453, #9638, #4336, #15149, #8186, #6019, #13347, #742, #6379 ),
 ( #4224, #15389, #17045, #13470, #620, #11560, #20730, #11675, #15499, #2529, #7947, #22536, #22652, #1432, #6845, #12025, #21548, #19289, #2879, #8654, #17860, #8299, #19403, #17400, #3126, #23366, #12503, #16078, #8540, #22889, #10225, #967, #23235, #6970, #17517, #5160, #8774, #3243, #2767, #14287, #15620, #6503, #12263, #10590, #10109, #13824, #13934, #14169, #1084, #10468, #5045, #21080, #4690, #8427, #12377, #15742, #23011, #6616, #21189, #4805, #17749, #12137, #23118, #1315, #3001, #10352, #21431, #19643, #17641, #1203, #15847, #6731, #21305, #14040, #4927, #19529, #15952, #11045, #16655, #231, #16191, #18443, #1792, #5512, #3362, #1559, #19883, #19990, #12845, #7340, #9256, #8896, #23603, #14645, #18333, #14409, #19760, #8, #14531, #21670, #3486, #21796, #10703, #17982, #9019, #1915, #12966, #18212, #3593, #5279, #16426, #21904, #16540, #20227, #23478, #116, #7090, #18094, #12622, #5758, #5402, #7448, #10821, #5633, #9140, #1676, #16312, #7217, #12740 ) ),
 .UNSPECIFIED., .F., .F., .F. ) 
 B_SPLINE_SURFACE_WITH_KNOTS ( ( 2, 2 ),
 ( 3, 2, 2, 2, 2, 2, 2, 2, 2, 2, 2, 2, 2, 2, 2, 2, 2, 2, 2, 2, 2, 2, 2, 2, 2, 2, 2, 2, 2, 2, 2, 2, 2, 2, 2, 2, 2, 2, 2, 2, 2, 2, 2, 2, 2, 2, 2, 2, 2, 2, 2, 2, 2, 2, 2, 2, 2, 2, 2, 2, 2, 2, 2, 2, 3 ),
 ( 0.000000000000000000, 1.000000000000000000 ),
 ( 0.000000000000000000, 0.01562500000000000000, 0.03125000000000000000, 0.04687500000000000000, 0.06250000000000000000, 0.07812500000000000000, 0.09375000000000000000, 0.1093750000000000000, 0.1250000000000000000, 0.1406250000000000000, 0.1562500000000000000, 0.1718750000000000000, 0.1875000000000000000, 0.2031250000000000000, 0.2187500000000000000, 0.2343750000000000000, 0.2500000000000000000, 0.2656250000000000000, 0.2812500000000000000, 0.2968750000000000000, 0.3125000000000000000, 0.3281250000000000000, 0.3437500000000000000, 0.3593750000000000000, 0.3750000000000000000, 0.3906250000000000000, 0.4062500000000000000, 0.4218750000000000000, 0.4375000000000000000, 0.4531250000000000000, 0.4687500000000000000, 0.4843750000000000000, 0.5000000000000000000, 0.5156250000000000000, 0.5312500000000000000, 0.5468750000000000000, 0.5625000000000000000, 0.5781250000000000000, 0.5937500000000000000, 0.6093750000000000000, 0.6250000000000000000, 0.6406250000000000000, 0.6562500000000000000, 0.6718750000000000000, 0.6875000000000000000, 0.7031250000000000000, 0.7187500000000000000, 0.7343750000000000000, 0.7500000000000000000, 0.7656250000000000000, 0.7812500000000000000, 0.7968750000000000000, 0.8125000000000000000, 0.8281250000000000000, 0.8437500000000000000, 0.8593750000000000000, 0.8750000000000000000, 0.8906250000000000000, 0.9062500000000000000, 0.9218750000000000000, 0.9375000000000000000, 0.9531250000000000000, 0.9687500000000000000, 0.9843750000000000000, 1.000000000000000000 ),
 .UNSPECIFIED. ) 
 GEOMETRIC_REPRESENTATION_ITEM ( )  RATIONAL_B_SPLINE_SURFACE ( (
 ( 1.000000000000000000, 0.9238795325112867385, 1.000000000000000000, 0.9238795325112867385, 1.000000000000000000, 0.9238795325112867385, 1.000000000000000000, 0.9238795325112867385, 1.000000000000000000, 0.9238795325112867385, 1.000000000000000000, 0.9238795325112867385, 1.000000000000000000, 0.9238795325112867385, 1.000000000000000000, 0.9238795325112867385, 1.000000000000000000, 0.9238795325112867385, 1.000000000000000000, 0.9238795325112867385, 1.000000000000000000, 0.9238795325112867385, 1.000000000000000000, 0.9238795325112867385, 1.000000000000000000, 0.9238795325112867385, 1.000000000000000000, 0.9238795325112867385, 1.000000000000000000, 0.9238795325112867385, 1.000000000000000000, 0.9238795325112867385, 1.000000000000000000, 0.9238795325112867385, 1.000000000000000000, 0.9238795325112867385, 1.000000000000000000, 0.9238795325112867385, 1.000000000000000000, 0.9238795325112867385, 1.000000000000000000, 0.9238795325112867385, 1.000000000000000000, 0.9238795325112867385, 1.000000000000000000, 0.9238795325112867385, 1.000000000000000000, 0.9238795325112867385, 1.000000000000000000, 0.9238795325112867385, 1.000000000000000000, 0.9238795325112867385, 1.000000000000000000, 0.9238795325112867385, 1.000000000000000000, 0.9238795325112867385, 1.000000000000000000, 0.9238795325112867385, 1.000000000000000000, 0.9238795325112867385, 1.000000000000000000, 0.9238795325112867385, 1.000000000000000000, 0.9238795325112867385, 1.000000000000000000, 0.9238795325112867385, 1.000000000000000000, 0.9238795325112867385, 1.000000000000000000, 0.9238795325112867385, 1.000000000000000000, 0.9238795325112867385, 1.000000000000000000, 0.9238795325112867385, 1.000000000000000000, 0.9238795325112867385, 1.000000000000000000, 0.9238795325112867385, 1.000000000000000000, 0.9238795325112867385, 1.000000000000000000, 0.9238795325112867385, 1.000000000000000000, 0.9238795325112867385, 1.000000000000000000, 0.9238795325112867385, 1.000000000000000000, 0.9238795325112867385, 1.000000000000000000, 0.9238795325112867385, 1.000000000000000000, 0.9238795325112867385, 1.000000000000000000, 0.9238795325112867385, 1.000000000000000000, 0.9238795325112867385, 1.000000000000000000, 0.9238795325112867385, 1.000000000000000000, 0.9238795325112867385, 1.000000000000000000, 0.9238795325112867385, 1.000000000000000000, 0.9238795325112867385, 1.000000000000000000, 0.9238795325112867385, 1.000000000000000000, 0.9238795325112867385, 1.000000000000000000, 0.9238795325112867385, 1.000000000000000000, 0.9238795325112867385, 1.000000000000000000, 0.9238795325112867385, 1.000000000000000000, 0.9238795325112867385, 1.000000000000000000, 0.9238795325112867385, 1.000000000000000000, 0.9238795325112867385, 1.000000000000000000, 0.9238795325112867385, 1.000000000000000000, 0.9238795325112867385, 1.000000000000000000, 0.9238795325112867385, 1.000000000000000000, 0.9238795325112867385, 1.000000000000000000),
 ( 1.000000000000000000, 0.9238795325112867385, 1.000000000000000000, 0.9238795325112867385, 1.000000000000000000, 0.9238795325112867385, 1.000000000000000000, 0.9238795325112867385, 1.000000000000000000, 0.9238795325112867385, 1.000000000000000000, 0.9238795325112867385, 1.000000000000000000, 0.9238795325112867385, 1.000000000000000000, 0.9238795325112867385, 1.000000000000000000, 0.9238795325112867385, 1.000000000000000000, 0.9238795325112867385, 1.000000000000000000, 0.9238795325112867385, 1.000000000000000000, 0.9238795325112867385, 1.000000000000000000, 0.9238795325112867385, 1.000000000000000000, 0.9238795325112867385, 1.000000000000000000, 0.9238795325112867385, 1.000000000000000000, 0.9238795325112867385, 1.000000000000000000, 0.9238795325112867385, 1.000000000000000000, 0.9238795325112867385, 1.000000000000000000, 0.9238795325112867385, 1.000000000000000000, 0.9238795325112867385, 1.000000000000000000, 0.9238795325112867385, 1.000000000000000000, 0.9238795325112867385, 1.000000000000000000, 0.9238795325112867385, 1.000000000000000000, 0.9238795325112867385, 1.000000000000000000, 0.9238795325112867385, 1.000000000000000000, 0.9238795325112867385, 1.000000000000000000, 0.9238795325112867385, 1.000000000000000000, 0.9238795325112867385, 1.000000000000000000, 0.9238795325112867385, 1.000000000000000000, 0.9238795325112867385, 1.000000000000000000, 0.9238795325112867385, 1.000000000000000000, 0.9238795325112867385, 1.000000000000000000, 0.9238795325112867385, 1.000000000000000000, 0.9238795325112867385, 1.000000000000000000, 0.9238795325112867385, 1.000000000000000000, 0.9238795325112867385, 1.000000000000000000, 0.9238795325112867385, 1.000000000000000000, 0.9238795325112867385, 1.000000000000000000, 0.9238795325112867385, 1.000000000000000000, 0.9238795325112867385, 1.000000000000000000, 0.9238795325112867385, 1.000000000000000000, 0.9238795325112867385, 1.000000000000000000, 0.9238795325112867385, 1.000000000000000000, 0.9238795325112867385, 1.000000000000000000, 0.9238795325112867385, 1.000000000000000000, 0.9238795325112867385, 1.000000000000000000, 0.9238795325112867385, 1.000000000000000000, 0.9238795325112867385, 1.000000000000000000, 0.9238795325112867385, 1.000000000000000000, 0.9238795325112867385, 1.000000000000000000, 0.9238795325112867385, 1.000000000000000000, 0.9238795325112867385, 1.000000000000000000, 0.9238795325112867385, 1.000000000000000000, 0.9238795325112867385, 1.000000000000000000, 0.9238795325112867385, 1.000000000000000000, 0.9238795325112867385, 1.000000000000000000, 0.9238795325112867385, 1.000000000000000000, 0.9238795325112867385, 1.000000000000000000, 0.9238795325112867385, 1.000000000000000000, 0.9238795325112867385, 1.000000000000000000, 0.9238795325112867385, 1.000000000000000000, 0.9238795325112867385, 1.000000000000000000, 0.9238795325112867385, 1.000000000000000000, 0.9238795325112867385, 1.000000000000000000) ) ) 
 REPRESENTATION_ITEM ( '' )  SURFACE ( )  );
#2075 = DIRECTION ( 'NONE',  ( 0.000000000000000000, 0.000000000000000000, -1.000000000000000000 ) ) ;
#2076 = ORIENTED_EDGE ( 'NONE', *, *, #21459, .F. ) ;
#2077 = DIRECTION ( 'NONE',  ( 0.000000000000000000, -1.000000000000000000, 0.000000000000000000 ) ) ;
#2078 = CARTESIAN_POINT ( 'NONE',  ( 3.458734125000001214, -1.432654583217639610, 1.425000001365597013 ) ) ;
#2079 = CARTESIAN_POINT ( 'NONE',  ( 68.70000000000000284, 7.499999999999996447, 14.99999999999999645 ) ) ;
#2080 = DIRECTION ( 'NONE',  ( -0.000000000000000000, -0.000000000000000000, 1.000000000000000000 ) ) ;
#2081 = AXIS2_PLACEMENT_3D ( 'NONE', #3226, #8886, #16300 ) ;
#2083 = DIRECTION ( 'NONE',  ( 0.000000000000000000, -0.5000000000000009992, -0.8660254037844380415 ) ) ;
#2082 = AXIS2_PLACEMENT_3D ( 'NONE', #15831, #16178, #3114 ) ;
#2084 = CARTESIAN_POINT ( 'NONE',  ( 53.75231816583844591, 7.219692298483957771, 17.87654654797633924 ) ) ;
#2085 = CIRCLE ( 'NONE', #10157, 2.055000000000000160 ) ;
#2086 = CARTESIAN_POINT ( 'NONE',  ( 2.445694354108820523, -2.445694354108820079, 0.1125000013655966247 ) ) ;
#2087 = CARTESIAN_POINT ( 'NONE',  ( -1.432654583217639166, 3.458734125000000770, 13.50000000136560452 ) ) ;
#2088 = EDGE_CURVE ( 'NONE', #16693, #10540, #5521, .T. ) ;
#2089 = CARTESIAN_POINT ( 'NONE',  ( -9.311853653233802319, -9.000000000000003553, 5.000000000000079936 ) ) ;
#2090 = CARTESIAN_POINT ( 'NONE',  ( -70.90000000109246514, 7.933012699999995476, 14.14382582708705094 ) ) ;
#2091 = CARTESIAN_POINT ( 'NONE',  ( 4.999999999999999112, -8.475820894092946034, -4.057423117305485327 ) ) ;
#2092 = ORIENTED_EDGE ( 'NONE', *, *, #15142, .F. ) ;
#2093 = CARTESIAN_POINT ( 'NONE',  ( 0.2615509004163102946, 3.991439731035835603, 2.039999999999998259 ) ) ;
#2094 = DIRECTION ( 'NONE',  ( 1.000000000000000000, -0.000000000000000000, -0.000000000000000000 ) ) ;
#2095 = CARTESIAN_POINT ( 'NONE',  ( 71.92500000163870766, 9.999999999999998224, 17.28349365000000049 ) ) ;
#2096 = ORIENTED_EDGE ( 'NONE', *, *, #11629, .F. ) ;
#2097 = ORIENTED_EDGE ( 'NONE', *, *, #11327, .T. ) ;
#2098 = DIRECTION ( 'NONE',  ( -0.000000000000000000, -0.000000000000000000, 1.000000000000000000 ) ) ;
#2099 = CARTESIAN_POINT ( 'NONE',  ( 57.28125000000000711, 8.343145750507600766, 11.00000000000000355 ) ) ;
#2100 = ORIENTED_EDGE ( 'NONE', *, *, #3101, .T. ) ;
#2101 = CARTESIAN_POINT ( 'NONE',  ( 4.999999999999999112, 0.000000000000000000, 0.000000000000000000 ) ) ;
#2102 = EDGE_LOOP ( 'NONE', ( #18696, #19564, #15462, #18201, #5418 ) ) ;
#2103 = CARTESIAN_POINT ( 'NONE',  ( 53.00231816583844591, 12.78030770151603868, 12.12345345202365188 ) ) ;
#2104 = AXIS2_PLACEMENT_3D ( 'NONE', #11305, #18579, #12014 ) ;
#2105 = AXIS2_PLACEMENT_3D ( 'NONE', #1625, #11114, #16144 ) ;
#2106 = CARTESIAN_POINT ( 'NONE',  ( 70.10000000109246798, 10.85617417291294551, 12.93301269999999370 ) ) ;
#2107 = DIRECTION ( 'NONE',  ( 1.000000000000000000, 0.000000000000000000, 0.000000000000000000 ) ) ;
#2108 = CARTESIAN_POINT ( 'NONE',  ( 70.40000000109247935, 12.06698730000000275, 14.14382582708705094 ) ) ;
#2109 = ORIENTED_EDGE ( 'NONE', *, *, #2492, .F. ) ;
#2110 = CARTESIAN_POINT ( 'NONE',  ( -1.656854249492379250, 4.000000000000000000, 18.93750000273119838 ) ) ;
#2111 = AXIS2_PLACEMENT_3D ( 'NONE', #14632, #9595, #21892 ) ;
#2112 = VECTOR ( 'NONE', #22635, 1000.000000000000000 ) ;
#2113 = CARTESIAN_POINT ( 'NONE',  ( 0.1129242967662022479, -9.000000000000001776, 10.00000000000008882 ) ) ;
#2114 = CARTESIAN_POINT ( 'NONE',  ( 54.99768183416157541, 12.87654654797631792, 12.21969229848393113 ) ) ;
#2115 = DIRECTION ( 'NONE',  ( -0.9396926207859107594, -0.3420201433256623291, 1.540743955509804830E-32 ) ) ;
#2116 = DIRECTION ( 'NONE',  ( 0.3420201433256622181, -0.9396926207859107594, 0.000000000000000000 ) ) ;
#2117 = CARTESIAN_POINT ( 'NONE',  ( -27.50000000000000711, 4.500000000000001776, -36.31025403784445871 ) ) ;
#2118 = CARTESIAN_POINT ( 'NONE',  ( -67.50000000109245946, 9.143825827087049163, 17.06698730000000097 ) ) ;
#2119 = AXIS2_PLACEMENT_3D ( 'NONE', #17968, #1304, #23002 ) ;
#2120 = CARTESIAN_POINT ( 'NONE',  ( -2.000000000000001776, 0.000000000000000000, 0.000000000000000000 ) ) ;
#2121 = ORIENTED_EDGE ( 'NONE', *, *, #2441, .F. ) ;
#2122 = CARTESIAN_POINT ( 'NONE',  ( 2.828427124746192067, -2.828427124746189847, 12.37500000000001066 ) ) ;
#2123 = AXIS2_PLACEMENT_3D ( 'NONE', #9081, #3309, #6922 ) ;
#2124 = CYLINDRICAL_SURFACE ( 'NONE', #19217, 4.000000000000001776 ) ;
#2125 = SURFACE_SIDE_STYLE ('',( #9118 ) ) ;
#2126 = EDGE_LOOP ( 'NONE', ( #8202, #17901 ) ) ;
#2127 = CARTESIAN_POINT ( 'NONE',  ( 3.803704290982252711, -5.309483803148803638, 1.219727444046192242E-16 ) ) ;
#2128 = FACE_OUTER_BOUND ( 'NONE', #8630, .T. ) ;
#2129 = CARTESIAN_POINT ( 'NONE',  ( 1.391697335622810172, 4.043246145443375461, -3.503898532754365913 ) ) ;
#2130 = CARTESIAN_POINT ( 'NONE',  ( -2.828427124746188515, -2.828427124746190735, 16.25000000273119838 ) ) ;
#2131 = VERTEX_POINT ( 'NONE', #3129 ) ;
#2132 = CARTESIAN_POINT ( 'NONE',  ( -69.80000000218494449, 9.999999999999998224, 12.49999999999999289 ) ) ;
#2133 = ORIENTED_EDGE ( 'NONE', *, *, #21624, .F. ) ;
#2134 = EDGE_CURVE ( 'NONE', #22281, #13130, #10470, .T. ) ;
#2135 = CARTESIAN_POINT ( 'NONE',  ( 26.67945438033275707, -11.25000000000000355, 10.00000000000008882 ) ) ;
#2136 = CARTESIAN_POINT ( 'NONE',  ( -2.828427124746189403, 2.828427124746190291, 15.87500000000001066 ) ) ;
#2137 = DIRECTION ( 'NONE',  ( -0.000000000000000000, 1.287488025362403787E-15, 1.000000000000000000 ) ) ;
#2138 = CARTESIAN_POINT ( 'NONE',  ( 4.999999999999999112, 5.222868219166995729, -9.680994141368715944 ) ) ;
#2139 = LINE ( 'NONE', #4067, #20538 ) ;
#2140 = CARTESIAN_POINT ( 'NONE',  ( 71.70000000109247651, 7.933012699999995476, 14.14382582708705094 ) ) ;
#2141 = ADVANCED_FACE ( 'NONE', ( #6972 ), #5163, .F. ) ;
#2142 = VERTEX_POINT ( 'NONE', #5281 ) ;
#2143 = DIRECTION ( 'NONE',  ( 0.000000000000000000, 0.5877852522924685852, 0.8090169943749506709 ) ) ;
#2144 = CARTESIAN_POINT ( 'NONE',  ( 1.236993788156008760E-15, 0.000000000000000000, 21.31370849898476649 ) ) ;
#2145 = CARTESIAN_POINT ( 'NONE',  ( 66.50000000109247367, 9.143825827087049163, 17.06698729999999742 ) ) ;
#2146 = CARTESIAN_POINT ( 'NONE',  ( -3.458734124999998993, 0.000000000000000000, 17.43750000136560274 ) ) ;
#2147 = CARTESIAN_POINT ( 'NONE',  ( 19.99999999999998934, 7.500000000000001776, -50.00000000000000000 ) ) ;
#2148 = CARTESIAN_POINT ( 'NONE',  ( -1.432654583217640498, 3.458734125000000770, -1.199999998634403431 ) ) ;
#2149 = CARTESIAN_POINT ( 'NONE',  ( -4.000000000000000888, 1.656854249492380804, 4.237499999999999822 ) ) ;
#2150 = CARTESIAN_POINT ( 'NONE',  ( 4.000000000000000888, -1.656854249492379694, -3.137499997268812901 ) ) ;
#2151 = CARTESIAN_POINT ( 'NONE',  ( -1.432654583217639610, -3.458734124999999882, 14.62500000136560629 ) ) ;
#2152 = DIRECTION ( 'NONE',  ( -0.000000000000000000, -0.000000000000000000, -1.000000000000000000 ) ) ;
#2153 = VERTEX_POINT ( 'NONE', #18097 ) ;
#2154 = CARTESIAN_POINT ( 'NONE',  ( -68.45000000109247651, 9.999999999999998224, 12.93301269999999192 ) ) ;
#2155 = EDGE_LOOP ( 'NONE', ( #7268, #12154, #13017, #8583 ) ) ;
#2156 = CARTESIAN_POINT ( 'NONE',  ( 57.84375000000000711, 8.343145750507638070, 19.00000000000000711 ) ) ;
#2157 = CARTESIAN_POINT ( 'NONE',  ( -69.90000000109246514, 9.143825827087049163, 17.06698729999999742 ) ) ;
#2158 = SHAPE_DEFINITION_REPRESENTATION ( #4559, #15757 ) ;
#2159 = ORIENTED_EDGE ( 'NONE', *, *, #13788, .F. ) ;
#2160 = DIRECTION ( 'NONE',  ( 0.000000000000000000, 0.000000000000000000, 1.000000000000000000 ) ) ;
#2161 = ORIENTED_EDGE ( 'NONE', *, *, #22966, .F. ) ;
#2162 = ADVANCED_FACE ( 'NONE', ( #1678 ), #18777, .T. ) ;
#2163 = ADVANCED_FACE ( 'NONE', ( #11826 ), #19328, .T. ) ;
#2164 = ORIENTED_EDGE ( 'NONE', *, *, #19940, .F. ) ;
#2165 = CARTESIAN_POINT ( 'NONE',  ( -3.458734124999999437, 0.000000000000000000, 16.68750000136560629 ) ) ;
#2166 = CARTESIAN_POINT ( 'NONE',  ( 55.87500000000000711, 7.878679656440349177, 12.87867965644035984 ) ) ;
#2167 = CIRCLE ( 'NONE', #15972, 4.000000000000000000 ) ;
#2168 = CARTESIAN_POINT ( 'NONE',  ( -69.00000000109247367, 7.933012699999995476, 15.85617417291294196 ) ) ;
#2169 = CARTESIAN_POINT ( 'NONE',  ( 69.85000000109248219, 7.933012699999995476, 14.99999999999999645 ) ) ;
#2170 = EDGE_CURVE ( 'NONE', #1668, #21207, #870, .T. ) ;
#2171 = EDGE_CURVE ( 'NONE', #21411, #21943, #12691, .T. ) ;
#2172 = CIRCLE ( 'NONE', #20530, 4.000000000000001776 ) ;
#2173 = CARTESIAN_POINT ( 'NONE',  ( -70.20000000109246230, 9.143825827087050939, 12.93301269999999370 ) ) ;
#2174 = CARTESIAN_POINT ( 'NONE',  ( 1.872352939448454495E-15, -3.458734125000000770, 12.93750000136560629 ) ) ;
#2175 = CARTESIAN_POINT ( 'NONE',  ( 5.000000000000000888, 0.000000000000000000, 0.000000000000000000 ) ) ;
#2176 = CARTESIAN_POINT ( 'NONE',  ( 59.02893183416158251, 11.17458954617365663, 18.02818770551464311 ) ) ;
#2177 = CARTESIAN_POINT ( 'NONE',  ( 71.75000000000001421, 8.964466094067221391, 17.49999999999996447 ) ) ;
#2178 = STYLED_ITEM ( 'NONE', ( #3945 ), #13661 ) ;
#2179 = CARTESIAN_POINT ( 'NONE',  ( 54.93750000000000711, 10.00000000000000711, 17.99999999999999645 ) ) ;
#2180 = CARTESIAN_POINT ( 'NONE',  ( -3.458734124999998105, 1.432654583217640276, 10.37500000136560629 ) ) ;
#2181 = CARTESIAN_POINT ( 'NONE',  ( 2.828427124746191179, 2.828427124746190291, 15.75000000273119660 ) ) ;
#2182 = CARTESIAN_POINT ( 'NONE',  ( 4.999999999999999112, 1.975651141462237970, 10.82112760146736896 ) ) ;
#2183 =( GEOMETRIC_REPRESENTATION_CONTEXT ( 3 ) GLOBAL_UNCERTAINTY_ASSIGNED_CONTEXT ( ( #11496 ) ) GLOBAL_UNIT_ASSIGNED_CONTEXT ( ( #16970, #18636, #7870 ) ) REPRESENTATION_CONTEXT ( 'NONE', 'WORKASPACE' ) );
#2184 = AXIS2_PLACEMENT_3D ( 'NONE', #13301, #20569, #13654 ) ;
#2185 = ORIENTED_EDGE ( 'NONE', *, *, #9823, .F. ) ;
#2186 = DIRECTION ( 'NONE',  ( 0.000000000000000000, 0.000000000000000000, -1.000000000000000000 ) ) ;
#2187 = CARTESIAN_POINT ( 'NONE',  ( -70.09999999999999432, 9.999999999999998224, 17.49999999999999645 ) ) ;
#2188 = ORIENTED_EDGE ( 'NONE', *, *, #19977, .F. ) ;
#2189 = CARTESIAN_POINT ( 'NONE',  ( 58.37268183416157541, 7.926799079670491466, 12.83056023321021755 ) ) ;
#2190 =( NAMED_UNIT ( * ) SI_UNIT ( $, .STERADIAN. ) SOLID_ANGLE_UNIT ( ) );
#2191 = CARTESIAN_POINT ( 'NONE',  ( 4.000000000000000000, 4.898587196589412829E-16, -3.074999997268812901 ) ) ;
#2192 = EDGE_CURVE ( 'NONE', #3210, #6908, #15443, .T. ) ;
#2193 = DIRECTION ( 'NONE',  ( -0.000000000000000000, -0.000000000000000000, -1.000000000000000000 ) ) ;
#2194 = VERTEX_POINT ( 'NONE', #3625 ) ;
#2195 = CARTESIAN_POINT ( 'NONE',  ( 1.656854249492381470, 4.000000000000000000, 13.68750000000001066 ) ) ;
#2196 = CARTESIAN_POINT ( 'NONE',  ( 39.24582498033275613, -11.25000000000000355, 10.00000000000008882 ) ) ;
#2197 = EDGE_CURVE ( 'NONE', #20481, #6488, #23638, .T. ) ;
#2198 = DIRECTION ( 'NONE',  ( -0.3420201433256622181, 0.9396926207859106484, 1.232595164407828100E-31 ) ) ;
#2199 = EDGE_LOOP ( 'NONE', ( #18134, #3021, #9568, #10063 ) ) ;
#2200 = VECTOR ( 'NONE', #14134, 1000.000000000000000 ) ;
#2201 = EDGE_CURVE ( 'NONE', #2045, #19611, #12396, .T. ) ;
#2202 = CARTESIAN_POINT ( 'NONE',  ( -3.458734125000000770, 0.000000000000000000, 1.987500001365596569 ) ) ;
#2203 = AXIS2_PLACEMENT_3D ( 'NONE', #4413, #11869, #6458 ) ;
#2204 = ADVANCED_FACE ( 'NONE', ( #10963 ), #18860, .T. ) ;
#2205 = CARTESIAN_POINT ( 'NONE',  ( 67.25000000000000000, 8.964466094067258695, 12.49999999999999289 ) ) ;
#2206 = DIRECTION ( 'NONE',  ( 0.000000000000000000, 0.000000000000000000, 1.000000000000000000 ) ) ;
#2207 = LINE ( 'NONE', #20162, #379 ) ;
#2208 = CARTESIAN_POINT ( 'NONE',  ( 53.37731816583844591, 7.123453452023657206, 12.21969229848395599 ) ) ;
#2209 = CARTESIAN_POINT ( 'NONE',  ( -2.117863837641485618E-16, 3.458734125000000770, 4.737500001365595459 ) ) ;
#2210 = CARTESIAN_POINT ( 'NONE',  ( 1.872352939448454495E-15, -3.458734125000000770, 16.93750000136560629 ) ) ;
#2211 = CARTESIAN_POINT ( 'NONE',  ( 21.00000000000000355, 0.000000000000000000, 2.055000000000000160 ) ) ;
#2212 = STYLED_ITEM ( 'NONE', ( #12501 ), #14766 ) ;
#2213 = LINE ( 'NONE', #10993, #18583 ) ;
#2214 = ORIENTED_EDGE ( 'NONE', *, *, #14206, .F. ) ;
#2215 = DIRECTION ( 'NONE',  ( 1.000000000000000000, -0.000000000000000000, -0.000000000000000000 ) ) ;
#2216 =( BOUNDED_CURVE ( )  B_SPLINE_CURVE ( 2, ( #21610, #8712, #10769, #18043, #10986, #1620, #12686, #19941, #3182 ),
 .UNSPECIFIED., .F., .T. ) 
 B_SPLINE_CURVE_WITH_KNOTS ( ( 3, 2, 2, 2, 3 ),
 ( 0.3125000000000002776, 0.3281250000000001665, 0.3437500000000001110, 0.3593750000000000000, 0.3749999999999998890 ),
 .UNSPECIFIED. ) 
 CURVE ( )  GEOMETRIC_REPRESENTATION_ITEM ( )  RATIONAL_B_SPLINE_CURVE ( ( 0.9999999999999986677, 0.9238795325112880708, 1.000000000000000000, 0.9238795325112867385, 1.000000000000000000, 0.9238795325112867385, 1.000000000000000000, 0.9238795325112872936, 0.9999999999999994449 ) ) 
 REPRESENTATION_ITEM ( '' )  );
#2217 = DIRECTION ( 'NONE',  ( -0.000000000000000000, 0.000000000000000000, -1.000000000000000000 ) ) ;
#2218 = CARTESIAN_POINT ( 'NONE',  ( -71.30000000109248504, 9.143825827087049163, 17.06698729999999742 ) ) ;
#2219 = ORIENTED_EDGE ( 'NONE', *, *, #12351, .F. ) ;
#2220 = CIRCLE ( 'NONE', #5290, 2.041999999999999815 ) ;
#2221 = ORIENTED_EDGE ( 'NONE', *, *, #1401, .F. ) ;
#2222 = AXIS2_PLACEMENT_3D ( 'NONE', #16703, #14936, #7737 ) ;
#2223 = DIRECTION ( 'NONE',  ( -0.000000000000000000, -1.000000000000000000, -0.000000000000000000 ) ) ;
#2224 = CARTESIAN_POINT ( 'NONE',  ( 52.68750000000000711, 9.999999999999978684, 10.99999999999999645 ) ) ;
#2225 = EDGE_LOOP ( 'NONE', ( #9888, #800, #7702, #7024 ) ) ;
#2226 = DIRECTION ( 'NONE',  ( 1.000000000000000000, 0.000000000000000000, 0.000000000000000000 ) ) ;
#2227 = EDGE_LOOP ( 'NONE', ( #12808, #7264, #9979, #16944 ) ) ;
#2228 = CARTESIAN_POINT ( 'NONE',  ( 52.90856816583843880, 13.97181229448534978, 13.27509460956196641 ) ) ;
#2229 = EDGE_CURVE ( 'NONE', #23499, #10887, #14567, .T. ) ;
#2230 = CARTESIAN_POINT ( 'NONE',  ( 66.25000000218494733, 8.964466094067258695, 17.50000000000000355 ) ) ;
#2231 = EDGE_CURVE ( 'NONE', #8785, #1325, #21496, .T. ) ;
#2232 = VECTOR ( 'NONE', #16777, 1000.000000000000000 ) ;
#2233 = CARTESIAN_POINT ( 'NONE',  ( 66.40000000000000568, 8.232233047033629347, 13.23223304703362402 ) ) ;
#2234 = CARTESIAN_POINT ( 'NONE',  ( 71.40000000109246514, 10.85617417291294551, 17.06698729999999742 ) ) ;
#2235 = PRODUCT_DEFINITION_SHAPE ( 'NONE', 'NONE',  #23713 ) ;
#2236 = VERTEX_POINT ( 'NONE', #7003 ) ;
#2237 = CARTESIAN_POINT ( 'NONE',  ( -2.828427124746188515, -2.828427124746190735, 13.25000000273119660 ) ) ;
#2238 = DIRECTION ( 'NONE',  ( -1.000000000000000000, 0.000000000000000000, 0.000000000000000000 ) ) ;
#2239 = VECTOR ( 'NONE', #10664, 1000.000000000000000 ) ;
#2240 = CARTESIAN_POINT ( 'NONE',  ( 59.81250000000000711, 14.00000000000000000, 14.99999999999997691 ) ) ;
#2241 = CARTESIAN_POINT ( 'NONE',  ( 2.916637777638891649, -2.156686440539167915, 2.039999999999998703 ) ) ;
#2242 = DIRECTION ( 'NONE',  ( -1.000000000000000000, 0.000000000000000000, -0.000000000000000000 ) ) ;
#2243 = DIRECTION ( 'NONE',  ( -1.000000000000000000, 0.000000000000000000, 0.000000000000000000 ) ) ;
#2244 = DIRECTION ( 'NONE',  ( 0.000000000000000000, 0.8090169943749444537, 0.5877852522924770229 ) ) ;
#2245 = LINE ( 'NONE', #14988, #22212 ) ;
#2246 = ORIENTED_EDGE ( 'NONE', *, *, #342, .T. ) ;
#2247 = CARTESIAN_POINT ( 'NONE',  ( -4.000000000000000000, -1.680117682357936904, -3.316611593218794951 ) ) ;
#2248 = DIRECTION ( 'NONE',  ( -0.000000000000000000, 1.000000000000000000, -0.000000000000000000 ) ) ;
#2249 = VECTOR ( 'NONE', #20228, 1000.000000000000000 ) ;
#2250 = ORIENTED_EDGE ( 'NONE', *, *, #23464, .T. ) ;
#2251 = CARTESIAN_POINT ( 'NONE',  ( 69.25000000218494733, 12.50000000000000000, 16.03553390593273775 ) ) ;
#2252 = CARTESIAN_POINT ( 'NONE',  ( -31.74999999999995737, 0.000000000000000000, 0.000000000000000000 ) ) ;
#2253 = DIRECTION ( 'NONE',  ( -1.000000000000000000, 0.000000000000000000, 0.000000000000000000 ) ) ;
#2254 = CARTESIAN_POINT ( 'NONE',  ( 5.200000000000002842, 0.000000000000000000, 2.500000000000000444 ) ) ;
#2255 = VERTEX_POINT ( 'NONE', #10851 ) ;
#2256 = CARTESIAN_POINT ( 'NONE',  ( 72.50000000000000000, 9.999999999999998224, 12.49999999999999289 ) ) ;
#2257 = VERTEX_POINT ( 'NONE', #3519 ) ;
#2258 = EDGE_CURVE ( 'NONE', #2257, #1597, #4239, .T. ) ;
#2259 =( BOUNDED_CURVE ( )  B_SPLINE_CURVE ( 2, ( #11515, #18535, #2122, #4168, #18787, #4524, #11860, #17237, #22962 ),
 .UNSPECIFIED., .F., .F. ) 
 B_SPLINE_CURVE_WITH_KNOTS ( ( 3, 2, 2, 2, 3 ),
 ( 0.7500000000000000000, 0.7624999999999999556, 0.7750000000000000222, 0.7874999999999999778, 0.8000000000000000444 ),
 .UNSPECIFIED. ) 
 CURVE ( )  GEOMETRIC_REPRESENTATION_ITEM ( )  RATIONAL_B_SPLINE_CURVE ( ( 1.000000000000000000, 0.9238795325112867385, 1.000000000000000000, 0.9238795325112867385, 1.000000000000000000, 0.9238795325112867385, 1.000000000000000000, 0.9238795325112867385, 1.000000000000000000 ) ) 
 REPRESENTATION_ITEM ( '' )  );
#2260 = CIRCLE ( 'NONE', #20616, 11.00000000000000000 ) ;
#2261 = DIRECTION ( 'NONE',  ( -0.000000000000000000, -0.000000000000000000, 1.000000000000000000 ) ) ;
#2262 = VECTOR ( 'NONE', #19534, 1000.000000000000000 ) ;
#2263 = CARTESIAN_POINT ( 'NONE',  ( -1.656854249492379250, 4.000000000000000000, 14.81250000000001066 ) ) ;
#2264 = FACE_OUTER_BOUND ( 'NONE', #6893, .T. ) ;
#2265 = DIRECTION ( 'NONE',  ( 0.3420201433256622181, 0.9396926207859107594, -6.162975822039141593E-32 ) ) ;
#2266 = DIRECTION ( 'NONE',  ( 0.3420201433256622736, 0.9396926207859106484, 0.000000000000000000 ) ) ;
#2267 = CARTESIAN_POINT ( 'NONE',  ( 71.15000000109246514, 11.46158073645647235, 13.53841926354352232 ) ) ;
#2268 = AXIS2_PLACEMENT_3D ( 'NONE', #1394, #16277, #8988 ) ;
#2269 = EDGE_LOOP ( 'NONE', ( #22214, #7129, #19850, #629 ) ) ;
#2270 = CIRCLE ( 'NONE', #14165, 4.000000000000001776 ) ;
#2271 = DIRECTION ( 'NONE',  ( 0.000000000000000000, 0.000000000000000000, -1.000000000000000000 ) ) ;
#2272 = PRODUCT_RELATED_PRODUCT_CATEGORY ( 'part', '', ( #2634 ) ) ;
#2273 = CARTESIAN_POINT ( 'NONE',  ( 1.025207404391860050E-15, 3.458734125000000770, 10.43750000136560629 ) ) ;
#2274 = CARTESIAN_POINT ( 'NONE',  ( 66.85000000109248219, 9.999999999999998224, 12.93301269999999192 ) ) ;
#2275 = CARTESIAN_POINT ( 'NONE',  ( 1.432654583217641164, 3.458734125000000326, 12.12500000136560629 ) ) ;
#2276 = LINE ( 'NONE', #17019, #23504 ) ;
#2277 = ADVANCED_FACE ( 'NONE', ( #23399 ), #5857, .T. ) ;
#2278 = CARTESIAN_POINT ( 'NONE',  ( 1.432654583217642275, -3.458734124999999882, -0.6999999986344028757 ) ) ;
#2279 = STYLED_ITEM ( 'NONE', ( #5346 ), #22323 ) ;
#2280 = CARTESIAN_POINT ( 'NONE',  ( 2.828427124746190735, -2.828427124746189847, 1.675000000000001155 ) ) ;
#2281 = CARTESIAN_POINT ( 'NONE',  ( 4.000000000000000888, 1.656854249492381248, 12.56250000000001243 ) ) ;
#2282 = CARTESIAN_POINT ( 'NONE',  ( 1.432654583217643163, -3.458734124999999437, 12.75000000136560629 ) ) ;
#2283 = CARTESIAN_POINT ( 'NONE',  ( 0.000000000000000000, 0.000000000000000000, 0.000000000000000000 ) ) ;
#2284 = ORIENTED_EDGE ( 'NONE', *, *, #17458, .F. ) ;
#2285 = CARTESIAN_POINT ( 'NONE',  ( -66.75000000109247367, 8.538419263543524096, 13.53841926354352054 ) ) ;
#2286 = EDGE_LOOP ( 'NONE', ( #2477, #16579, #11571, #7358 ) ) ;
#2287 = CARTESIAN_POINT ( 'NONE',  ( 59.15625000000002132, 6.000000000000004441, 16.65685424949239390 ) ) ;
#2288 = CARTESIAN_POINT ( 'NONE',  ( -72.00000000109245946, 12.06698730000000275, 14.14382582708705094 ) ) ;
#2289 = APPLICATION_PROTOCOL_DEFINITION ( 'draft international standard', 'automotive_design', 1998, #21519 ) ;
#2290 = EDGE_LOOP ( 'NONE', ( #6796, #9438 ) ) ;
#2291 = CARTESIAN_POINT ( 'NONE',  ( -4.000000000000000000, 0.000000000000000000, 1.425000002731187765 ) ) ;
#2292 = ORIENTED_EDGE ( 'NONE', *, *, #13935, .T. ) ;
#2293 = AXIS2_PLACEMENT_3D ( 'NONE', #6505, #6148, #15743 ) ;
#2294 = AXIS2_PLACEMENT_3D ( 'NONE', #20762, #4367, #2689 ) ;
#2295 = ORIENTED_EDGE ( 'NONE', *, *, #5529, .T. ) ;
#2296 = CARTESIAN_POINT ( 'NONE',  ( 3.458734125000002546, -1.432654583217639610, 15.12500000136560807 ) ) ;
#2297 = CARTESIAN_POINT ( 'NONE',  ( 56.15625000000002132, 7.000000000000003553, 16.24264068711929099 ) ) ;
#2298 = VECTOR ( 'NONE', #6085, 1000.000000000000000 ) ;
#2299 = CARTESIAN_POINT ( 'NONE',  ( -66.65000000109247935, 7.933012699999995476, 14.99999999999999645 ) ) ;
#2300 = VECTOR ( 'NONE', #14417, 1000.000000000000000 ) ;
#2301 = CARTESIAN_POINT ( 'NONE',  ( 67.95000000109247651, 11.46158073645647235, 16.46158073645647235 ) ) ;
#2302 = CARTESIAN_POINT ( 'NONE',  ( -68.05000000109247082, 12.06698730000000097, 14.99999999999999645 ) ) ;
#2303 = DIRECTION ( 'NONE',  ( 0.000000000000000000, 1.000000000000000000, -1.287488025362403787E-15 ) ) ;
#2304 = CARTESIAN_POINT ( 'NONE',  ( 58.46643183416158251, 7.028187705514638672, 13.68930817193508531 ) ) ;
#2305 = DIRECTION ( 'NONE',  ( -0.000000000000000000, -0.000000000000000000, 1.000000000000000000 ) ) ;
#2306 = B_SPLINE_CURVE_WITH_KNOTS ( 'NONE', 3,
 ( #18528, #18304, #12934, #10906 ),
 .UNSPECIFIED., .F., .F.,
 ( 4, 4 ),
 ( 0.000000000000000000, 0.1324062220596828598 ),
 .UNSPECIFIED. ) ;
#2307 = EDGE_CURVE ( 'NONE', #16726, #19572, #20022, .T. ) ;
#2308 = CARTESIAN_POINT ( 'NONE',  ( -3.458734125000000770, 0.000000000000000000, 4.987500001365595459 ) ) ;
#2309 = ADVANCED_FACE ( 'NONE', ( #1825 ), #5623, .T. ) ;
#2310 = CARTESIAN_POINT ( 'NONE',  ( -2.445694354108818303, -2.445694354108820523, 10.56250000136560452 ) ) ;
#2311 = CARTESIAN_POINT ( 'NONE',  ( -2.828427124746189403, 2.828427124746190291, 15.00000000273119660 ) ) ;
#2312 = DIRECTION ( 'NONE',  ( -7.087422195345011518E-32, -1.000000000000000000, 0.000000000000000000 ) ) ;
#2313 = AXIS2_PLACEMENT_3D ( 'NONE', #21472, #23163, #23405 ) ;
#2314 = VERTEX_POINT ( 'NONE', #6363 ) ;
#2315 = CARTESIAN_POINT ( 'NONE',  ( 0.02511973781850649831, -4.877415612947427981, -3.751298745799844792 ) ) ;
#2316 = ORIENTED_EDGE ( 'NONE', *, *, #6174, .F. ) ;
#2317 = CARTESIAN_POINT ( 'NONE',  ( 58.93518183416157541, 9.931948859054372747, 17.99999999999999645 ) ) ;
#2318 = CARTESIAN_POINT ( 'NONE',  ( 6.353591512924457348E-16, -3.458734125000000326, 2.987500001365597235 ) ) ;
#2319 = EDGE_CURVE ( 'NONE', #17824, #14427, #19163, .T. ) ;
#2320 = CARTESIAN_POINT ( 'NONE',  ( -5.434916218090833695, -4.367703157927336655, -0.2578475836320747172 ) ) ;
#2321 = ORIENTED_EDGE ( 'NONE', *, *, #20642, .F. ) ;
#2322 = CARTESIAN_POINT ( 'NONE',  ( 2.828427124746191179, 2.828427124746190291, 12.62500000000001066 ) ) ;
#2323 = FACE_OUTER_BOUND ( 'NONE', #9677, .T. ) ;
#2324 = CYLINDRICAL_SURFACE ( 'NONE', #17527, 4.000000000000001776 ) ;
#2325 = ORIENTED_EDGE ( 'NONE', *, *, #15515, .F. ) ;
#2326 = CARTESIAN_POINT ( 'NONE',  ( -70.75000000218496155, 12.50000000000000000, 13.96446609406725869 ) ) ;
#2327 = FACE_OUTER_BOUND ( 'NONE', #11099, .T. ) ;
#2328 = VECTOR ( 'NONE', #5880, 1000.000000000000114 ) ;
#2329 = LINE ( 'NONE', #7976, #16409 ) ;
#2330 = CARTESIAN_POINT ( 'NONE',  ( 69.64999999999999147, 8.964466094067258695, 12.49999999999999289 ) ) ;
#2331 = CARTESIAN_POINT ( 'NONE',  ( -3.250000000000004441, 5.629165124598849879, -3.700000000000000178 ) ) ;
#2332 = CARTESIAN_POINT ( 'NONE',  ( 19.99999999999999289, -9.999999999999964473, -20.00000000000000355 ) ) ;
#2333 = CARTESIAN_POINT ( 'NONE',  ( 58.06481816583843170, 6.999999999999998224, 15.06805114094563436 ) ) ;
#2334 = EDGE_CURVE ( 'NONE', #892, #3058, #1642, .T. ) ;
#2335 = CARTESIAN_POINT ( 'NONE',  ( -3.458734125000000326, -1.432654583217642497, 5.050000001365596347 ) ) ;
#2336 = CARTESIAN_POINT ( 'NONE',  ( 2.445694354108822299, -2.445694354108820079, 15.06250000136560452 ) ) ;
#2337 = DIRECTION ( 'NONE',  ( 0.000000000000000000, 0.000000000000000000, -1.000000000000000000 ) ) ;
#2338 = CARTESIAN_POINT ( 'NONE',  ( -72.25000000109247367, 9.999999999999998224, 17.06698730000000097 ) ) ;
#2339 = CARTESIAN_POINT ( 'NONE',  ( -69.84999999999999432, 12.50000000000000000, 13.96446609406725692 ) ) ;
#2340 = VERTEX_POINT ( 'NONE', #20829 ) ;
#2341 = DIRECTION ( 'NONE',  ( 0.000000000000000000, 8.881784197001252323E-16, 1.000000000000000000 ) ) ;
#2342 = CARTESIAN_POINT ( 'NONE',  ( -1.656854249492381248, -3.999999999999999112, 4.612500002731188431 ) ) ;
#2343 = CARTESIAN_POINT ( 'NONE',  ( -71.40000000109249356, 7.933012699999995476, 15.85617417291294196 ) ) ;
#2344 = EDGE_CURVE ( 'NONE', #1931, #4288, #12005, .T. ) ;
#2345 = VERTEX_POINT ( 'NONE', #17498 ) ;
#2346 = EDGE_CURVE ( 'NONE', #6899, #6515, #719, .T. ) ;
#2347 = ORIENTED_EDGE ( 'NONE', *, *, #6296, .T. ) ;
#2348 = FILL_AREA_STYLE_COLOUR ( '', #21300 ) ;
#2349 = DIRECTION ( 'NONE',  ( -1.000000000000000000, 0.000000000000000000, -0.000000000000000000 ) ) ;
#2350 = ORIENTED_EDGE ( 'NONE', *, *, #22694, .T. ) ;
#2351 = LINE ( 'NONE', #15558, #6078 ) ;
#2352 = UNCERTAINTY_MEASURE_WITH_UNIT (LENGTH_MEASURE( 1.000000000000000082E-05 ), #20701, 'distance_accuracy_value', 'NONE');
#2353 = CARTESIAN_POINT ( 'NONE',  ( 71.95000000109247651, 11.46158073645647235, 16.46158073645647235 ) ) ;
#2354 = DIRECTION ( 'NONE',  ( -1.000000000000000000, -7.703719777548943412E-32, 0.000000000000000000 ) ) ;
#2355 = CARTESIAN_POINT ( 'NONE',  ( 71.50000000109247367, 9.143825827087049163, 17.06698729999999742 ) ) ;
#2356 = ORIENTED_EDGE ( 'NONE', *, *, #16601, .F. ) ;
#2357 = CARTESIAN_POINT ( 'NONE',  ( 1.656854249492384135, -3.999999999999999112, 12.43750000273119838 ) ) ;
#2358 = CARTESIAN_POINT ( 'NONE',  ( 21.00000000000000355, 2.789133085058097101E-16, -2.055000000000000160 ) ) ;
#2359 =( BOUNDED_CURVE ( )  B_SPLINE_CURVE ( 2, ( #14711, #16604, #9205, #14827, #183, #9429, #427, #11480, #5818 ),
 .UNSPECIFIED., .F., .F. ) 
 B_SPLINE_CURVE_WITH_KNOTS ( ( 3, 2, 2, 2, 3 ),
 ( 0.2999999999999999889, 0.3125000000000000000, 0.3250000000000000111, 0.3375000000000000222, 0.3499999999999999778 ),
 .UNSPECIFIED. ) 
 CURVE ( )  GEOMETRIC_REPRESENTATION_ITEM ( )  RATIONAL_B_SPLINE_CURVE ( ( 1.000000000000000000, 0.9238795325112867385, 1.000000000000000000, 0.9238795325112867385, 1.000000000000000000, 0.9238795325112867385, 1.000000000000000000, 0.9238795325112867385, 1.000000000000000000 ) ) 
 REPRESENTATION_ITEM ( '' )  );
#2360 = CARTESIAN_POINT ( 'NONE',  ( 55.37268183416157541, 7.219692298483935566, 12.12345345202367675 ) ) ;
#2361 = CARTESIAN_POINT ( 'NONE',  ( 71.75000000218496155, 11.03553390593273953, 17.50000000000000355 ) ) ;
#2362 = CARTESIAN_POINT ( 'NONE',  ( 3.458734125000001214, 1.432654583217640498, 17.00000000136560629 ) ) ;
#2363 = CARTESIAN_POINT ( 'NONE',  ( 4.000000000000000888, 4.898587196589412829E-16, 10.62500000273119660 ) ) ;
#2364 = CARTESIAN_POINT ( 'NONE',  ( -67.20000000109246230, 12.06698729999999919, 14.14382582708705094 ) ) ;
#2365 = FACE_OUTER_BOUND ( 'NONE', #7378, .T. ) ;
#2366 = VERTEX_POINT ( 'NONE', #13451 ) ;
#2367 = EDGE_CURVE ( 'NONE', #462, #18141, #3932, .T. ) ;
#2368 = CARTESIAN_POINT ( 'NONE',  ( -3.999999999998910649, -1.658469974638591804, -3.531532913075256186 ) ) ;
#2369 = DIRECTION ( 'NONE',  ( -1.000000000000000000, 0.000000000000000000, 0.000000000000000000 ) ) ;
#2370 = EDGE_CURVE ( 'NONE', #19770, #5947, #8556, .T. ) ;
#2371 = EDGE_CURVE ( 'NONE', #14828, #6681, #13805, .T. ) ;
#2372 = VERTEX_POINT ( 'NONE', #4318 ) ;
#2373 = DIRECTION ( 'NONE',  ( 0.000000000000000000, 0.000000000000000000, 1.000000000000000000 ) ) ;
#2374 = DIRECTION ( 'NONE',  ( 0.000000000000000000, 0.000000000000000000, -1.000000000000000000 ) ) ;
#2375 = DIRECTION ( 'NONE',  ( 1.000000000000000000, 7.703719777548943412E-32, 0.000000000000000000 ) ) ;
#2376 = AXIS2_PLACEMENT_3D ( 'NONE', #11979, #11861, #2723 ) ;
#2377 = FACE_OUTER_BOUND ( 'NONE', #1830, .T. ) ;
#2378 = ORIENTED_EDGE ( 'NONE', *, *, #2925, .T. ) ;
#2379 = CARTESIAN_POINT ( 'NONE',  ( 4.623144047065554041, 4.836380039389420737, -3.593844378834468056 ) ) ;
#2380 = ORIENTED_EDGE ( 'NONE', *, *, #4128, .T. ) ;
#2381 = CARTESIAN_POINT ( 'NONE',  ( 4.000000000000000888, 1.656854249492381248, 18.68750000273119483 ) ) ;
#2382 = CARTESIAN_POINT ( 'NONE',  ( -3.999999999999999112, 1.656854249492380804, 12.93750000000001243 ) ) ;
#2383 = CYLINDRICAL_SURFACE ( 'NONE', #10385, 11.00000000000000000 ) ;
#2384 = LINE ( 'NONE', #4421, #6863 ) ;
#2385 = CARTESIAN_POINT ( 'NONE',  ( 40.96287359071656908, -8.974600000000002353, 5.000000000000079936 ) ) ;
#2386 = CARTESIAN_POINT ( 'NONE',  ( 71.20000000109246230, 12.06698729999999919, 14.14382582708705094 ) ) ;
#2387 = ORIENTED_EDGE ( 'NONE', *, *, #22388, .F. ) ;
#2388 = CARTESIAN_POINT ( 'NONE',  ( 4.350941807883109469, 4.993536075455421219, -0.06682554136337783002 ) ) ;
#2389 = DIRECTION ( 'NONE',  ( 1.000000000000000000, 0.000000000000000000, 0.000000000000000000 ) ) ;
#2390 = CARTESIAN_POINT ( 'NONE',  ( 67.35000000109248219, 8.538419263543522320, 16.46158073645647235 ) ) ;
#2391 = CARTESIAN_POINT ( 'NONE',  ( 3.458734125000002102, -1.432654583217639610, 13.87500000136560452 ) ) ;
#2392 = DIRECTION ( 'NONE',  ( 0.000000000000000000, 0.000000000000000000, 1.000000000000000000 ) ) ;
#2393 = CARTESIAN_POINT ( 'NONE',  ( 3.458734125000001214, -1.432654583217639610, -2.574999998634404541 ) ) ;
#2395 = ADVANCED_FACE ( 'NONE', ( #11772 ), #21061, .T. ) ;
#2394 = CARTESIAN_POINT ( 'NONE',  ( -2.828427124746189403, -2.828427124746190735, 2.425000000000001599 ) ) ;
#2396 = DIRECTION ( 'NONE',  ( -1.000000000000000000, 0.000000000000000000, 0.000000000000000000 ) ) ;
#2397 = CARTESIAN_POINT ( 'NONE',  ( 2.445694354108821855, -2.445694354108820079, 10.81250000136560452 ) ) ;
#2398 = PLANE ( 'NONE',  #23329 ) ;
#2399 =( BOUNDED_CURVE ( )  B_SPLINE_CURVE ( 2, ( #5639, #2150, #18567, #22270, #2032, #20713, #17023, #9728, #4317 ),
 .UNSPECIFIED., .F., .F. ) 
 B_SPLINE_CURVE_WITH_KNOTS ( ( 3, 2, 2, 2, 3 ),
 ( 0.8499999999999999778, 0.8625000000000000444, 0.8750000000000000000, 0.8874999999999999556, 0.9000000000000000222 ),
 .UNSPECIFIED. ) 
 CURVE ( )  GEOMETRIC_REPRESENTATION_ITEM ( )  RATIONAL_B_SPLINE_CURVE ( ( 1.000000000000000000, 0.9238795325112867385, 1.000000000000000000, 0.9238795325112867385, 1.000000000000000000, 0.9238795325112867385, 1.000000000000000000, 0.9238795325112867385, 1.000000000000000000 ) ) 
 REPRESENTATION_ITEM ( '' )  );
#2400 = ORIENTED_EDGE ( 'NONE', *, *, #4433, .F. ) ;
#2401 = DIRECTION ( 'NONE',  ( -0.000000000000000000, 1.000000000000000000, -0.000000000000000000 ) ) ;
#2402 = VERTEX_POINT ( 'NONE', #11544 ) ;
#2403 = CARTESIAN_POINT ( 'NONE',  ( 55.96875000000000000, 5.999999999999987566, 13.34314575050763452 ) ) ;
#2404 = CARTESIAN_POINT ( 'NONE',  ( -70.95000000109247651, 8.538419263543524096, 13.53841926354352054 ) ) ;
#2405 = PRODUCT_CONTEXT ( 'NONE', #10237, 'mechanical' ) ;
#2406 = EDGE_LOOP ( 'NONE', ( #2495, #956 ) ) ;
#2407 = CARTESIAN_POINT ( 'NONE',  ( 2.000000000000001776, 8.013782491920513601E-16, -6.543750000000017053 ) ) ;
#2408 = VERTEX_POINT ( 'NONE', #13678 ) ;
#2409 = ORIENTED_EDGE ( 'NONE', *, *, #10292, .F. ) ;
#2410 = CARTESIAN_POINT ( 'NONE',  ( -1.432654583217639832, -3.458734125000000326, 16.87500000136560629 ) ) ;
#2411 = CARTESIAN_POINT ( 'NONE',  ( 57.93750000000000000, 10.00000000000000711, 17.99999999999999645 ) ) ;
#2412 = AXIS2_PLACEMENT_3D ( 'NONE', #20205, #21999, #18423 ) ;
#2413 = CARTESIAN_POINT ( 'NONE',  ( -67.20000000109247651, 10.85617417291294551, 17.06698729999999742 ) ) ;
#2414 = VECTOR ( 'NONE', #8432, 1000.000000000000000 ) ;
#2415 = CARTESIAN_POINT ( 'NONE',  ( 70.25000000109247367, 12.06698730000000097, 14.99999999999999645 ) ) ;
#2416 = CARTESIAN_POINT ( 'NONE',  ( -66.30000000109247082, 10.85617417291294551, 12.93301269999999370 ) ) ;
#2417 = DIRECTION ( 'NONE',  ( 0.000000000000000000, 0.000000000000000000, -1.000000000000000000 ) ) ;
#2418 = CARTESIAN_POINT ( 'NONE',  ( 59.77893183416158962, 8.825410453826341595, 11.97181229448535511 ) ) ;
#2419 = CARTESIAN_POINT ( 'NONE',  ( 4.999999999999999112, 9.680994141368771011, 5.222868219166890036 ) ) ;
#2420 = CARTESIAN_POINT ( 'NONE',  ( -1.432654583217641164, -3.458734125000000326, 2.175000001365597679 ) ) ;
#2421 = CARTESIAN_POINT ( 'NONE',  ( -3.974344831685191280E-13, 4.796734841935104576, -3.721909803043223608 ) ) ;
#2422 = CARTESIAN_POINT ( 'NONE',  ( -2.828427124746189403, 2.828427124746190291, 17.00000000273119838 ) ) ;
#2423 = CARTESIAN_POINT ( 'NONE',  ( 68.70000000000000284, 7.499999999999996447, 14.99999999999999645 ) ) ;
#2424 = ORIENTED_EDGE ( 'NONE', *, *, #479, .T. ) ;
#2425 = CARTESIAN_POINT ( 'NONE',  ( 4.999999999999997335, 0.000000000000000000, 4.250000000000000000 ) ) ;
#2426 = ORIENTED_EDGE ( 'NONE', *, *, #14982, .T. ) ;
#2427 = CARTESIAN_POINT ( 'NONE',  ( 60.99768183416157541, 12.16943976678977535, 12.92679907967048614 ) ) ;
#2428 = CARTESIAN_POINT ( 'NONE',  ( 1.432654583217642275, -3.458734124999999437, 1.050000001365596791 ) ) ;
#2429 = VECTOR ( 'NONE', #16406, 1000.000000000000000 ) ;
#2430 = CARTESIAN_POINT ( 'NONE',  ( 3.458734125000000326, 4.235727675282971730E-16, 0.2375000013655967357 ) ) ;
#2431 = ORIENTED_EDGE ( 'NONE', *, *, #22949, .T. ) ;
#2432 = CARTESIAN_POINT ( 'NONE',  ( 2.828427124746192067, -2.828427124746189847, 13.37500000000001243 ) ) ;
#2433 = DIRECTION ( 'NONE',  ( 7.087422195345011518E-32, 1.000000000000000000, 0.000000000000000000 ) ) ;
#2434 = DIRECTION ( 'NONE',  ( 0.000000000000000000, 0.000000000000000000, 1.000000000000000000 ) ) ;
#2435 = ORIENTED_EDGE ( 'NONE', *, *, #3000, .T. ) ;
#2436 = EDGE_CURVE ( 'NONE', #10458, #7419, #22869, .T. ) ;
#2437 = CARTESIAN_POINT ( 'NONE',  ( -70.40000000218495302, 7.499999999999996447, 14.99999999999999645 ) ) ;
#2438 = CARTESIAN_POINT ( 'NONE',  ( -2.445694354108819635, -2.445694354108820967, -1.887499998634403431 ) ) ;
#2439 = DIRECTION ( 'NONE',  ( -1.000000000000000000, 0.000000000000000000, 0.000000000000000000 ) ) ;
#2440 = CARTESIAN_POINT ( 'NONE',  ( 66.79999999999999716, 11.76776695296636888, 16.76776695296636532 ) ) ;
#2441 = EDGE_CURVE ( 'NONE', #23104, #9739, #12007, .T. ) ;
#2442 = CARTESIAN_POINT ( 'NONE',  ( -3.999999999999998224, -1.656854249492383024, 11.06250000000001066 ) ) ;
#2443 = CARTESIAN_POINT ( 'NONE',  ( 70.65000000109247935, 7.933012699999995476, 14.99999999999999645 ) ) ;
#2444 = CARTESIAN_POINT ( 'NONE',  ( 9.537702246766199821, -9.000000000000005329, 5.000000000000079936 ) ) ;
#2445 = CARTESIAN_POINT ( 'NONE',  ( 57.12731816583843170, 12.16943976678978601, 17.07320092032949432 ) ) ;
#2446 = CARTESIAN_POINT ( 'NONE',  ( 6.353591512924457348E-16, -3.458734125000000770, 5.237500001365596347 ) ) ;
#2447 = CARTESIAN_POINT ( 'NONE',  ( 3.458734125000001658, 4.235727675282972223E-16, 14.18750000136560629 ) ) ;
#2448 = DIRECTION ( 'NONE',  ( 0.3420201433256622181, -0.9396926207859107594, 0.000000000000000000 ) ) ;
#2449 = CARTESIAN_POINT ( 'NONE',  ( -71.35000000109246798, 11.46158073645647235, 16.46158073645647235 ) ) ;
#2450 = CARTESIAN_POINT ( 'NONE',  ( 0.000000000000000000, 0.000000000000000000, 0.000000000000000000 ) ) ;
#2451 = ORIENTED_EDGE ( 'NONE', *, *, #3652, .F. ) ;
#2452 = CARTESIAN_POINT ( 'NONE',  ( 3.869372803233808611, -9.000000000000003553, 5.000000000000079936 ) ) ;
#2453 = CARTESIAN_POINT ( 'NONE',  ( 1.656854249492380360, 4.000000000000000000, 4.112500002731187543 ) ) ;
#2454 = CARTESIAN_POINT ( 'NONE',  ( -71.60000000109246798, 9.143825827087050939, 12.93301269999999370 ) ) ;
#2455 = ORIENTED_EDGE ( 'NONE', *, *, #11790, .T. ) ;
#2456 = ORIENTED_EDGE ( 'NONE', *, *, #10434, .F. ) ;
#2457 = CARTESIAN_POINT ( 'NONE',  ( 15.00195451966726523, -11.25000000000000355, 5.000000000000079936 ) ) ;
#2458 = CYLINDRICAL_SURFACE ( 'NONE', #8723, 6.499999999999999112 ) ;
#2459 = ORIENTED_EDGE ( 'NONE', *, *, #13057, .T. ) ;
#2460 = CARTESIAN_POINT ( 'NONE',  ( 3.436319922986518449, -2.634841920959471562, -3.531542292954761741 ) ) ;
#2461 = EDGE_CURVE ( 'NONE', #2366, #11492, #17025, .T. ) ;
#2462 = ADVANCED_FACE ( 'NONE', ( #4786 ), #15845, .T. ) ;
#2463 = CARTESIAN_POINT ( 'NONE',  ( 68.75000000109247367, 11.46158073645647235, 16.46158073645647235 ) ) ;
#2464 = VECTOR ( 'NONE', #9085, 1000.000000000000000 ) ;
#2465 = AXIS2_PLACEMENT_3D ( 'NONE', #13620, #6547, #19333 ) ;
#2466 = CARTESIAN_POINT ( 'NONE',  ( 71.20000000109246230, 12.06698730000000275, 14.14382582708705094 ) ) ;
#2467 = VECTOR ( 'NONE', #12355, 1000.000000000000000 ) ;
#2468 = ADVANCED_FACE ( 'NONE', ( #5141 ), #5875, .T. ) ;
#2469 = VERTEX_POINT ( 'NONE', #8634 ) ;
#2470 = EDGE_CURVE ( 'NONE', #12570, #16559, #7071, .T. ) ;
#2471 = DIRECTION ( 'NONE',  ( -1.000000000000000000, -0.000000000000000000, -0.000000000000000000 ) ) ;
#2472 = CARTESIAN_POINT ( 'NONE',  ( 53.15625000000001421, 6.000000000000004441, 16.65685424949239390 ) ) ;
#2473 = CARTESIAN_POINT ( 'NONE',  ( -2.000000000000001776, 0.000000000000000000, 0.000000000000000000 ) ) ;
#2474 = CARTESIAN_POINT ( 'NONE',  ( 1.432654583217643163, -3.458734124999999437, 17.75000000136560274 ) ) ;
#2475 = DIRECTION ( 'NONE',  ( -0.9396926207859107594, -0.3420201433256623291, 1.540743955509804830E-32 ) ) ;
#2476 = CARTESIAN_POINT ( 'NONE',  ( -67.10000000109246798, 10.85617417291294551, 12.93301269999999192 ) ) ;
#2477 = ORIENTED_EDGE ( 'NONE', *, *, #19719, .T. ) ;
#2478 = DIRECTION ( 'NONE',  ( 0.000000000000000000, 0.000000000000000000, 1.000000000000000000 ) ) ;
#2479 = ORIENTED_EDGE ( 'NONE', *, *, #3099, .F. ) ;
#2480 = CARTESIAN_POINT ( 'NONE',  ( -3.251184232703611343, 2.330193357860981695, -3.674599999999999866 ) ) ;
#2481 = DIRECTION ( 'NONE',  ( 1.000000000000000000, 7.703719777548943412E-32, 0.000000000000000000 ) ) ;
#2482 = ORIENTED_EDGE ( 'NONE', *, *, #16675, .T. ) ;
#2483 = LINE ( 'NONE', #10064, #17040 ) ;
#2484 = CARTESIAN_POINT ( 'NONE',  ( -1.656854249492379472, 4.000000000000000000, 14.93750000273119660 ) ) ;
#2485 = LINE ( 'NONE', #11982, #4039 ) ;
#2486 = VECTOR ( 'NONE', #9908, 1000.000000000000000 ) ;
#2487 = CARTESIAN_POINT ( 'NONE',  ( -1.393473772768861529, 3.889074120053769512, 9.929297958371448019 ) ) ;
#2488 = ORIENTED_EDGE ( 'NONE', *, *, #12030, .F. ) ;
#2489 = LINE ( 'NONE', #19017, #21338 ) ;
#2490 = ORIENTED_EDGE ( 'NONE', *, *, #8240, .F. ) ;
#2491 = CARTESIAN_POINT ( 'NONE',  ( 4.000000000000000888, 1.656854249492381248, 17.56250000000001066 ) ) ;
#2492 = EDGE_CURVE ( 'NONE', #15511, #10158, #580, .T. ) ;
#2493 = CARTESIAN_POINT ( 'NONE',  ( 2.828427124746191179, 2.828427124746190291, 12.62500000000001066 ) ) ;
#2494 = CARTESIAN_POINT ( 'NONE',  ( -5.968343123267130679, 4.059728990630802947, -3.296662375310749127 ) ) ;
#2495 = ORIENTED_EDGE ( 'NONE', *, *, #15806, .T. ) ;
#2496 = CARTESIAN_POINT ( 'NONE',  ( 0.000000000000000000, 0.000000000000000000, 0.000000000000000000 ) ) ;
#2497 =( BOUNDED_CURVE ( )  B_SPLINE_CURVE ( 2, ( #9362, #16775, #17128, #4189, #22625, #15231, #9608, #11401, #22376, #11279, #8040, #2140, #7799, #2499, #7560, #704, #18681, #13195, #11532, #20460, #229, #2386, #2267, #15356, #6228, #13548, #22258, #7913, #4308, #5754, #16900, #9835, #475, #18803, #9715, #2019, #5987, #4068, #3946, #9475, #15117, #22499, #20816, #14882, #13313, #16651, #17012, #4423, #11759, #20340, #354, #7688, #22137, #13085, #18555, #20583, #588, #6108, #13440, #15006, #20702, #11646, #18911, #5871, #17367, #2617, #10079, #10438, #21160, #15924, #8513, #2849, #4659, #15706, #4545, #1282, #19149, #1054, #19499, #826, #17720, #6586, #8390, #935, #13791, #23087, #19372, #19261, #8619, #23201, #6814, #15589, #1172, #21272, #22739, #10198, #3096, #17487, #4774, #12110, #19029, #14135, #21401, #5018, #9960, #17255, #8158, #2966, #15468, #6350, #13664, #6469, #6698, #8273, #10319, #4895, #20925, #11880, #2738, #12231, #22855, #21047, #22981, #11994, #17607, #14013, #13901, #15815, #14258 ),
 .UNSPECIFIED., .F., .F. ) 
 B_SPLINE_CURVE_WITH_KNOTS ( ( 3, 2, 2, 2, 2, 2, 2, 2, 2, 2, 2, 2, 2, 2, 2, 2, 2, 2, 2, 2, 2, 2, 2, 2, 2, 2, 2, 2, 2, 2, 2, 2, 2, 2, 2, 2, 2, 2, 2, 2, 2, 2, 2, 2, 2, 2, 2, 2, 2, 2, 2, 2, 2, 2, 2, 2, 2, 2, 2, 2, 2, 2, 2, 2, 3 ),
 ( 0.000000000000000000, 0.01562500000000000000, 0.03125000000000000000, 0.04687500000000000000, 0.06250000000000000000, 0.07812500000000000000, 0.09375000000000000000, 0.1093750000000000000, 0.1250000000000000000, 0.1406250000000000000, 0.1562500000000000000, 0.1718750000000000000, 0.1875000000000000000, 0.2031250000000000000, 0.2187500000000000000, 0.2343750000000000000, 0.2500000000000000000, 0.2656250000000000000, 0.2812500000000000000, 0.2968750000000000000, 0.3125000000000000000, 0.3281250000000000000, 0.3437500000000000000, 0.3593750000000000000, 0.3750000000000000000, 0.3906250000000000000, 0.4062500000000000000, 0.4218750000000000000, 0.4375000000000000000, 0.4531250000000000000, 0.4687500000000000000, 0.4843750000000000000, 0.5000000000000000000, 0.5156250000000000000, 0.5312500000000000000, 0.5468750000000000000, 0.5625000000000000000, 0.5781250000000000000, 0.5937500000000000000, 0.6093750000000000000, 0.6250000000000000000, 0.6406250000000000000, 0.6562500000000000000, 0.6718750000000000000, 0.6875000000000000000, 0.7031250000000000000, 0.7187500000000000000, 0.7343750000000000000, 0.7500000000000000000, 0.7656250000000000000, 0.7812500000000000000, 0.7968750000000000000, 0.8125000000000000000, 0.8281250000000000000, 0.8437500000000000000, 0.8593750000000000000, 0.8750000000000000000, 0.8906250000000000000, 0.9062500000000000000, 0.9218750000000000000, 0.9375000000000000000, 0.9531250000000000000, 0.9687500000000000000, 0.9843750000000000000, 1.000000000000000000 ),
 .UNSPECIFIED. ) 
 CURVE ( )  GEOMETRIC_REPRESENTATION_ITEM ( )  RATIONAL_B_SPLINE_CURVE ( ( 1.000000000000000000, 0.9238795325112867385, 1.000000000000000000, 0.9238795325112867385, 1.000000000000000000, 0.9238795325112867385, 1.000000000000000000, 0.9238795325112867385, 1.000000000000000000, 0.9238795325112867385, 1.000000000000000000, 0.9238795325112867385, 1.000000000000000000, 0.9238795325112867385, 1.000000000000000000, 0.9238795325112867385, 1.000000000000000000, 0.9238795325112867385, 1.000000000000000000, 0.9238795325112867385, 1.000000000000000000, 0.9238795325112867385, 1.000000000000000000, 0.9238795325112867385, 1.000000000000000000, 0.9238795325112867385, 1.000000000000000000, 0.9238795325112867385, 1.000000000000000000, 0.9238795325112867385, 1.000000000000000000, 0.9238795325112867385, 1.000000000000000000, 0.9238795325112867385, 1.000000000000000000, 0.9238795325112867385, 1.000000000000000000, 0.9238795325112867385, 1.000000000000000000, 0.9238795325112867385, 1.000000000000000000, 0.9238795325112867385, 1.000000000000000000, 0.9238795325112867385, 1.000000000000000000, 0.9238795325112867385, 1.000000000000000000, 0.9238795325112867385, 1.000000000000000000, 0.9238795325112867385, 1.000000000000000000, 0.9238795325112867385, 1.000000000000000000, 0.9238795325112867385, 1.000000000000000000, 0.9238795325112867385, 1.000000000000000000, 0.9238795325112867385, 1.000000000000000000, 0.9238795325112867385, 1.000000000000000000, 0.9238795325112867385, 1.000000000000000000, 0.9238795325112867385, 1.000000000000000000, 0.9238795325112867385, 1.000000000000000000, 0.9238795325112867385, 1.000000000000000000, 0.9238795325112867385, 1.000000000000000000, 0.9238795325112867385, 1.000000000000000000, 0.9238795325112867385, 1.000000000000000000, 0.9238795325112867385, 1.000000000000000000, 0.9238795325112867385, 1.000000000000000000, 0.9238795325112867385, 1.000000000000000000, 0.9238795325112867385, 1.000000000000000000, 0.9238795325112867385, 1.000000000000000000, 0.9238795325112867385, 1.000000000000000000, 0.9238795325112867385, 1.000000000000000000, 0.9238795325112867385, 1.000000000000000000, 0.9238795325112867385, 1.000000000000000000, 0.9238795325112867385, 1.000000000000000000, 0.9238795325112867385, 1.000000000000000000, 0.9238795325112867385, 1.000000000000000000, 0.9238795325112867385, 1.000000000000000000, 0.9238795325112867385, 1.000000000000000000, 0.9238795325112867385, 1.000000000000000000, 0.9238795325112867385, 1.000000000000000000, 0.9238795325112867385, 1.000000000000000000, 0.9238795325112867385, 1.000000000000000000, 0.9238795325112867385, 1.000000000000000000, 0.9238795325112867385, 1.000000000000000000, 0.9238795325112867385, 1.000000000000000000, 0.9238795325112867385, 1.000000000000000000, 0.9238795325112867385, 1.000000000000000000, 0.9238795325112867385, 1.000000000000000000, 0.9238795325112867385, 1.000000000000000000, 0.9238795325112867385, 1.000000000000000000, 0.9238795325112867385, 1.000000000000000000 ) ) 
 REPRESENTATION_ITEM ( '' )  );
#2498 = DIRECTION ( 'NONE',  ( 0.000000000000000000, 0.000000000000000000, 1.000000000000000000 ) ) ;
#2499 = CARTESIAN_POINT ( 'NONE',  ( 71.60000000109246798, 7.933012699999995476, 15.85617417291294196 ) ) ;
#2500 = VERTEX_POINT ( 'NONE', #14024 ) ;
#2501 = EDGE_CURVE ( 'NONE', #946, #5741, #9719, .T. ) ;
#2502 = CONICAL_SURFACE ( 'NONE', #1350, 4.000000000000000000, 0.8911886515913786111 ) ;
#2503 = CARTESIAN_POINT ( 'NONE',  ( -4.000000000000000000, 2.309401076758498483, -3.433295621305379353 ) ) ;
#2504 = CARTESIAN_POINT ( 'NONE',  ( 4.999999999999999112, -9.680994141368730155, -5.222868219166961978 ) ) ;
#2505 = CARTESIAN_POINT ( 'NONE',  ( 68.90000000109246514, 12.06698730000000275, 15.85617417291294196 ) ) ;
#2506 = CARTESIAN_POINT ( 'NONE',  ( 3.458734125000002102, -1.432654583217639610, 14.87500000136560807 ) ) ;
#2507 = CARTESIAN_POINT ( 'NONE',  ( -2.000000000000001776, 0.000000000000000000, 0.000000000000000000 ) ) ;
#2508 = DIRECTION ( 'NONE',  ( -0.000000000000000000, 0.000000000000000000, 1.000000000000000000 ) ) ;
#2509 = ORIENTED_EDGE ( 'NONE', *, *, #21073, .T. ) ;
#2510 = CARTESIAN_POINT ( 'NONE',  ( -2.828427124746189403, -2.828427124746190735, -0.5749999999999974021 ) ) ;
#2511 = DIRECTION ( 'NONE',  ( 0.000000000000000000, 0.000000000000000000, 1.000000000000000000 ) ) ;
#2512 = CARTESIAN_POINT ( 'NONE',  ( -3.458734124999998993, 1.432654583217640276, 10.37500000136560629 ) ) ;
#2513 = CYLINDRICAL_SURFACE ( 'NONE', #8412, 8.073750000000021743 ) ;
#2514 = VECTOR ( 'NONE', #14476, 1000.000000000000000 ) ;
#2515 = ORIENTED_EDGE ( 'NONE', *, *, #17282, .T. ) ;
#2516 = CARTESIAN_POINT ( 'NONE',  ( 1.656854249492381470, 4.000000000000000000, 15.81250000273119660 ) ) ;
#2517 = ORIENTED_EDGE ( 'NONE', *, *, #19916, .F. ) ;
#2518 = CARTESIAN_POINT ( 'NONE',  ( 59.90625000000000711, 13.99999999999999289, 13.34314575050759544 ) ) ;
#2519 = CARTESIAN_POINT ( 'NONE',  ( -68.30000000109247082, 9.143825827087049163, 17.06698729999999742 ) ) ;
#2520 = VERTEX_POINT ( 'NONE', #19623 ) ;
#2521 = CARTESIAN_POINT ( 'NONE',  ( -2.828427124746190291, 2.828427124746190291, -1.699999997268811569 ) ) ;
#2522 = EDGE_LOOP ( 'NONE', ( #4591, #11690 ) ) ;
#2523 = EDGE_LOOP ( 'NONE', ( #11872, #13867, #11518, #21273 ) ) ;
#2524 = CARTESIAN_POINT ( 'NONE',  ( -1.432654583217639832, -3.458734125000000326, 17.87500000136560274 ) ) ;
#2525 = CARTESIAN_POINT ( 'NONE',  ( 57.09375000000000711, 11.24264068711927322, 11.99999999999998934 ) ) ;
#2526 = CARTESIAN_POINT ( 'NONE',  ( -68.95000000109247651, 8.538419263543522320, 16.46158073645647235 ) ) ;
#2527 = CARTESIAN_POINT ( 'NONE',  ( 68.55000000109247082, 11.46158073645647235, 13.53841926354352232 ) ) ;
#2528 = EDGE_CURVE ( 'NONE', #4844, #5170, #10805, .T. ) ;
#2529 = CARTESIAN_POINT ( 'NONE',  ( -72.05000000000001137, 8.964466094067258695, 12.49999999999999289 ) ) ;
#2530 = CARTESIAN_POINT ( 'NONE',  ( 4.999999999999999112, 9.314797388894893615, 5.239665997526921082 ) ) ;
#2531 = CARTESIAN_POINT ( 'NONE',  ( 58.56018183416157541, 7.000000000000000000, 14.93194885905437097 ) ) ;
#2532 = PLANE ( 'NONE',  #5477 ) ;
#2533 = CARTESIAN_POINT ( 'NONE',  ( 3.458734125000001214, -1.432654583217639610, 4.425000001365595459 ) ) ;
#2534 = CARTESIAN_POINT ( 'NONE',  ( 3.458734125000002102, -1.432654583217639610, 11.87500000136560629 ) ) ;
#2535 = CARTESIAN_POINT ( 'NONE',  ( 9.920644283265380691E-16, 4.000000000000000000, 11.87500000273119660 ) ) ;
#2536 = DIRECTION ( 'NONE',  ( 1.224646799147353207E-16, -0.000000000000000000, 1.000000000000000000 ) ) ;
#2537 = VERTEX_POINT ( 'NONE', #6599 ) ;
#2538 = CARTESIAN_POINT ( 'NONE',  ( -3.999999999999999112, 1.656854249492380582, 17.06250000273120193 ) ) ;
#2539 = ORIENTED_EDGE ( 'NONE', *, *, #16677, .T. ) ;
#2540 = CARTESIAN_POINT ( 'NONE',  ( 56.49768183416158962, 12.16943976678977535, 12.92679907967048614 ) ) ;
#2541 = CARTESIAN_POINT ( 'NONE',  ( 2.445694354108820079, 2.445694354108820523, 3.362500001365597679 ) ) ;
#2542 = CARTESIAN_POINT ( 'NONE',  ( 2.445694354108820079, 2.445694354108820523, -0.6374999986344040970 ) ) ;
#2543 = EDGE_LOOP ( 'NONE', ( #16291, #1568, #17086, #21048 ) ) ;
#2544 = CARTESIAN_POINT ( 'NONE',  ( 4.000000000000001776, -1.656854249492379694, 14.43750000000001066 ) ) ;
#2545 = DIRECTION ( 'NONE',  ( 0.000000000000000000, 0.000000000000000000, 1.000000000000000000 ) ) ;
#2546 = DIRECTION ( 'NONE',  ( -1.000000000000000000, -7.703719777548943412E-32, 0.000000000000000000 ) ) ;
#2547 = ORIENTED_EDGE ( 'NONE', *, *, #21664, .F. ) ;
#2548 = AXIS2_PLACEMENT_3D ( 'NONE', #12304, #8821, #17785 ) ;
#2549 = CARTESIAN_POINT ( 'NONE',  ( -71.60000000218494165, 12.50000000000000000, 14.99999999999999645 ) ) ;
#2550 = CARTESIAN_POINT ( 'NONE',  ( 6.353591512924457348E-16, -3.458734125000000770, -1.762499998634403209 ) ) ;
#2551 = FACE_OUTER_BOUND ( 'NONE', #2227, .T. ) ;
#2552 = CARTESIAN_POINT ( 'NONE',  ( -70.95000000000000284, 8.964466094067294222, 17.50000000000003908 ) ) ;
#2553 = AXIS2_PLACEMENT_3D ( 'NONE', #3660, #7517, #22210 ) ;
#2554 = CARTESIAN_POINT ( 'NONE',  ( 68.95000000109247651, 8.538419263543522320, 16.46158073645647235 ) ) ;
#2555 = AXIS2_PLACEMENT_3D ( 'NONE', #23498, #20011, #9160 ) ;
#2556 = LINE ( 'NONE', #9904, #5357 ) ;
#2557 = CARTESIAN_POINT ( 'NONE',  ( 56.84606816583843880, 8.825410453826357582, 18.02818770551464667 ) ) ;
#2558 = CARTESIAN_POINT ( 'NONE',  ( -1.432654583217640276, 3.458734125000000326, -3.449999998634403653 ) ) ;
#2559 = CARTESIAN_POINT ( 'NONE',  ( -2.445694354108819191, 2.445694354108820523, 10.56250000136560629 ) ) ;
#2560 = PLANE ( 'NONE',  #21397 ) ;
#2561 = CARTESIAN_POINT ( 'NONE',  ( -71.90000000109246514, 10.85617417291294551, 12.93301269999999192 ) ) ;
#2562 = EDGE_CURVE ( 'NONE', #14122, #19663, #21172, .T. ) ;
#2563 = LINE ( 'NONE', #9910, #22680 ) ;
#2564 = CYLINDRICAL_SURFACE ( 'NONE', #2465, 4.000000000000001776 ) ;
#2565 = ORIENTED_EDGE ( 'NONE', *, *, #23408, .T. ) ;
#2566 = CARTESIAN_POINT ( 'NONE',  ( 118.3095189484530181, 14.69846310392956745, 35.82846581308617573 ) ) ;
#2567 = DIRECTION ( 'NONE',  ( -0.000000000000000000, -1.000000000000000000, -0.000000000000000000 ) ) ;
#2568 = FACE_OUTER_BOUND ( 'NONE', #18804, .T. ) ;
#2569 = ORIENTED_EDGE ( 'NONE', *, *, #8771, .T. ) ;
#2570 = APPLICATION_CONTEXT ( 'automotive_design' ) ;
#2571 = ORIENTED_EDGE ( 'NONE', *, *, #22356, .T. ) ;
#2572 = AXIS2_PLACEMENT_3D ( 'NONE', #7687, #15005, #2266 ) ;
#2573 = CARTESIAN_POINT ( 'NONE',  ( 4.000000000000000888, -1.656854249492379694, 1.862500002731187765 ) ) ;
#2574 = EDGE_CURVE ( 'NONE', #14091, #14025, #23666, .T. ) ;
#2575 = CARTESIAN_POINT ( 'NONE',  ( 52.03125000000000711, 11.65685424949239923, 18.99999999999998934 ) ) ;
#2576 = ORIENTED_EDGE ( 'NONE', *, *, #16881, .T. ) ;
#2577 = DIRECTION ( 'NONE',  ( 1.000000000000000000, -0.000000000000000000, -0.000000000000000000 ) ) ;
#2578 = VECTOR ( 'NONE', #1980, 1000.000000000000000 ) ;
#2579 = AXIS2_PLACEMENT_3D ( 'NONE', #15914, #1163, #12339 ) ;
#2580 = UNCERTAINTY_MEASURE_WITH_UNIT (LENGTH_MEASURE( 1.000000000000000082E-05 ), #9292, 'distance_accuracy_value', 'NONE');
#2581 = CARTESIAN_POINT ( 'NONE',  ( 68.10000000109246798, 9.143825827087049163, 17.06698729999999742 ) ) ;
#2582 = CONICAL_SURFACE ( 'NONE', #22482, 2.055000000000000160, 0.7853981633974639331 ) ;
#2583 = CARTESIAN_POINT ( 'NONE',  ( 67.20000000109247651, 12.06698730000000275, 14.14382582708705094 ) ) ;
#2584 = VERTEX_POINT ( 'NONE', #23099 ) ;
#2585 = AXIS2_PLACEMENT_3D ( 'NONE', #6585, #4894, #17606 ) ;
#2586 = CARTESIAN_POINT ( 'NONE',  ( -20.00000000000000711, 1.500000000000003109, -17.32050807568893092 ) ) ;
#2587 = CARTESIAN_POINT ( 'NONE',  ( 56.25000000000000711, 7.171572875253819923, 17.82842712474619873 ) ) ;
#2588 = CARTESIAN_POINT ( 'NONE',  ( -0.5316568767328819778, -7.198601258566901251, -3.296662375310746462 ) ) ;
#2589 = CARTESIAN_POINT ( 'NONE',  ( 66.80000000218494449, 12.50000000000000000, 14.99999999999999645 ) ) ;
#2590 = CARTESIAN_POINT ( 'NONE',  ( 50.00000000000000000, -10.00000000000001599, 34.11836509645782201 ) ) ;
#2591 = VECTOR ( 'NONE', #22429, 1000.000000000000000 ) ;
#2592 = EDGE_CURVE ( 'NONE', #158, #13665, #7029, .T. ) ;
#2593 = AXIS2_PLACEMENT_3D ( 'NONE', #10126, #6394, #21449 ) ;
#2594 = CYLINDRICAL_SURFACE ( 'NONE', #1300, 2.500000000000007550 ) ;
#2595 = VERTEX_POINT ( 'NONE', #10451 ) ;
#2596 = PLANE ( 'NONE',  #8049 ) ;
#2597 = EDGE_CURVE ( 'NONE', #5522, #17674, #3025, .T. ) ;
#2598 = FACE_OUTER_BOUND ( 'NONE', #23227, .T. ) ;
#2599 = LINE ( 'NONE', #19007, #14646 ) ;
#2600 = ORIENTED_EDGE ( 'NONE', *, *, #14803, .F. ) ;
#2601 = CARTESIAN_POINT ( 'NONE',  ( -66.20000000218495018, 9.999999999999998224, 17.49999999999999645 ) ) ;
#2602 = LINE ( 'NONE', #9947, #21336 ) ;
#2603 = CARTESIAN_POINT ( 'NONE',  ( 4.999999999999999112, -8.475820894092946034, -4.057423117305485327 ) ) ;
#2604 = EDGE_CURVE ( 'NONE', #2635, #12546, #23461, .T. ) ;
#2605 = CARTESIAN_POINT ( 'NONE',  ( -70.60000000218494165, 9.999999999999998224, 12.49999999999999289 ) ) ;
#2606 = EDGE_LOOP ( 'NONE', ( #11060, #17510, #10663, #17349 ) ) ;
#2607 = DIRECTION ( 'NONE',  ( 1.000000000000000000, 7.703719777548943412E-32, 0.000000000000000000 ) ) ;
#2608 = ORIENTED_EDGE ( 'NONE', *, *, #4965, .F. ) ;
#2609 = CIRCLE ( 'NONE', #5678, 2.500000000000000444 ) ;
#2610 = CARTESIAN_POINT ( 'NONE',  ( 72.05000000109247082, 9.999999999999998224, 17.06698730000000097 ) ) ;
#2611 = CARTESIAN_POINT ( 'NONE',  ( 35.27605445928345063, -8.974600000000002353, 5.000000000000079936 ) ) ;
#2612 = CARTESIAN_POINT ( 'NONE',  ( 71.60000000218494165, 12.50000000000000000, 14.99999999999999645 ) ) ;
#2613 = VECTOR ( 'NONE', #6455, 1000.000000000000000 ) ;
#2614 = CARTESIAN_POINT ( 'NONE',  ( 0.000000000000000000, -8.734705317681623171, -0.4999240074895356933 ) ) ;
#2615 = AXIS2_PLACEMENT_3D ( 'NONE', #468, #11525, #4301 ) ;
#2616 = CARTESIAN_POINT ( 'NONE',  ( -1.656854249492379472, 4.000000000000000000, 11.81250000000001066 ) ) ;
#2617 = CARTESIAN_POINT ( 'NONE',  ( 69.00000000109245946, 10.85617417291294551, 17.06698730000000097 ) ) ;
#2618 = ORIENTED_EDGE ( 'NONE', *, *, #7801, .F. ) ;
#2619 = CARTESIAN_POINT ( 'NONE',  ( 72.50000000000000000, 9.999999999999998224, 12.49999999999999289 ) ) ;
#2620 = EDGE_CURVE ( 'NONE', #6127, #11172, #14510, .T. ) ;
#2621 = DIRECTION ( 'NONE',  ( -0.000000000000000000, -0.000000000000000000, 1.000000000000000000 ) ) ;
#2622 = VECTOR ( 'NONE', #15472, 1000.000000000000000 ) ;
#2623 = CARTESIAN_POINT ( 'NONE',  ( 70.80000000109245661, 7.933012699999995476, 15.85617417291294196 ) ) ;
#2624 = CARTESIAN_POINT ( 'NONE',  ( -1.432654583217639610, -3.458734124999999882, 12.62500000136560629 ) ) ;
#2625 = DIRECTION ( 'NONE',  ( 1.000000000000000000, 0.000000000000000000, 0.000000000000000000 ) ) ;
#2626 = VECTOR ( 'NONE', #4607, 1000.000000000000000 ) ;
#2627 = LINE ( 'NONE', #596, #20681 ) ;
#2628 = ORIENTED_EDGE ( 'NONE', *, *, #2925, .F. ) ;
#2629 = CARTESIAN_POINT ( 'NONE',  ( -2.449293598294706907E-16, 4.000000000000000000, 3.050000000000002487 ) ) ;
#2630 = ADVANCED_FACE ( 'NONE', ( #3687 ), #3926, .F. ) ;
#2631 = CARTESIAN_POINT ( 'NONE',  ( 9.920644283265380691E-16, 4.000000000000000000, 15.75000000000001066 ) ) ;
#2632 = DIRECTION ( 'NONE',  ( 0.000000000000000000, 0.000000000000000000, -1.000000000000000000 ) ) ;
#2633 = DIRECTION ( 'NONE',  ( 0.000000000000000000, -1.000000000000000000, 0.000000000000000000 ) ) ;
#2634 = PRODUCT ( 'Machined Body Housing', 'Machined Body Housing', '', ( #1929 ) ) ;
#2635 = VERTEX_POINT ( 'NONE', #3578 ) ;
#2636 = CARTESIAN_POINT ( 'NONE',  ( -65.80000000109247082, 7.933012699999995476, 15.85617417291294196 ) ) ;
#2637 = ORIENTED_EDGE ( 'NONE', *, *, #18137, .T. ) ;
#2638 = CARTESIAN_POINT ( 'NONE',  ( -67.05000000109247082, 9.999999999999998224, 12.93301269999999192 ) ) ;
#2639 = VECTOR ( 'NONE', #1564, 1000.000000000000114 ) ;
#2640 = ADVANCED_FACE ( 'NONE', ( #1775 ), #23078, .T. ) ;
#2641 = ORIENTED_EDGE ( 'NONE', *, *, #15276, .T. ) ;
#2642 = CARTESIAN_POINT ( 'NONE',  ( 65.97500000054623115, 9.999999999999998224, 17.28349365000000049 ) ) ;
#2643 = VERTEX_POINT ( 'NONE', #11381 ) ;
#2644 = EDGE_CURVE ( 'NONE', #21534, #19492, #98, .T. ) ;
#2645 = AXIS2_PLACEMENT_3D ( 'NONE', #12216, #6930, #10427 ) ;
#2646 =( BOUNDED_CURVE ( )  B_SPLINE_CURVE ( 2, ( #1975, #18162, #5702, #16722, #16851, #185, #23670, #7286, #21859 ),
 .UNSPECIFIED., .F., .F. ) 
 B_SPLINE_CURVE_WITH_KNOTS ( ( 3, 2, 2, 2, 3 ),
 ( 0.6999999999999999556, 0.7125000000000000222, 0.7249999999999999778, 0.7375000000000000444, 0.7500000000000000000 ),
 .UNSPECIFIED. ) 
 CURVE ( )  GEOMETRIC_REPRESENTATION_ITEM ( )  RATIONAL_B_SPLINE_CURVE ( ( 1.000000000000000000, 0.9238795325112867385, 1.000000000000000000, 0.9238795325112867385, 1.000000000000000000, 0.9238795325112867385, 1.000000000000000000, 0.9238795325112867385, 1.000000000000000000 ) ) 
 REPRESENTATION_ITEM ( '' )  );
#2647 = ORIENTED_EDGE ( 'NONE', *, *, #10100, .F. ) ;
#2648 = CARTESIAN_POINT ( 'NONE',  ( -1.432654583217639832, -3.458734125000000326, 14.87500000136560807 ) ) ;
#2649 = DIRECTION ( 'NONE',  ( 0.000000000000000000, -1.000000000000000000, 0.000000000000000000 ) ) ;
#2650 = AXIS2_PLACEMENT_3D ( 'NONE', #8276, #2970, #4899 ) ;
#2651 = CARTESIAN_POINT ( 'NONE',  ( -66.15000000109247935, 11.46158073645647235, 13.53841926354352232 ) ) ;
#2652 = CARTESIAN_POINT ( 'NONE',  ( 69.45000000109247651, 12.06698730000000097, 14.99999999999999645 ) ) ;
#2653 = AXIS2_PLACEMENT_3D ( 'NONE', #3257, #7106, #23251 ) ;
#2654 = CARTESIAN_POINT ( 'NONE',  ( -66.40000000109247935, 12.06698730000000275, 14.14382582708705094 ) ) ;
#2655 = CONICAL_SURFACE ( 'NONE', #21006, 6.543750000000017053, 0.4459949661726622105 ) ;
#2656 = CARTESIAN_POINT ( 'NONE',  ( 6.499999999999999112, 0.000000000000000000, 1.734723475976807094E-15 ) ) ;
#2657 = CARTESIAN_POINT ( 'NONE',  ( 57.90393183416158251, 13.02818770551463778, 13.82541045382633982 ) ) ;
#2658 = DIRECTION ( 'NONE',  ( 0.000000000000000000, 0.000000000000000000, 1.000000000000000000 ) ) ;
#2659 = CARTESIAN_POINT ( 'NONE',  ( 3.458734125000001214, -1.432654583217639610, 2.425000001365597679 ) ) ;
#2660 = CARTESIAN_POINT ( 'NONE',  ( 71.39999999999999147, 11.76776695296636888, 13.23223304703362579 ) ) ;
#2661 = CARTESIAN_POINT ( 'NONE',  ( -1.656854249492380138, -3.999999999999999112, 11.31250000273119660 ) ) ;
#2662 = VECTOR ( 'NONE', #10669, 1000.000000000000114 ) ;
#2663 = CARTESIAN_POINT ( 'NONE',  ( 4.999999999999999112, -4.729683950898817102, -7.360373001730970977 ) ) ;
#2664 = AXIS2_PLACEMENT_3D ( 'NONE', #4636, #11970, #22954 ) ;
#2665 = ORIENTED_EDGE ( 'NONE', *, *, #12495, .T. ) ;
#2666 = CARTESIAN_POINT ( 'NONE',  ( 2.499999999999999556, 5.222868219166856285, 9.680994141368792327 ) ) ;
#2667 = ORIENTED_EDGE ( 'NONE', *, *, #14055, .T. ) ;
#2668 = CARTESIAN_POINT ( 'NONE',  ( 59.31018183416157541, 12.99999999999999822, 15.06805114094562192 ) ) ;
#2669 = DIRECTION ( 'NONE',  ( 1.000000000000000000, 0.000000000000000000, 0.000000000000000000 ) ) ;
#2670 = CARTESIAN_POINT ( 'NONE',  ( 2.445694354108820523, -2.445694354108820079, 3.112500001365597679 ) ) ;
#2671 = EDGE_CURVE ( 'NONE', #23515, #16003, #20324, .T. ) ;
#2672 = CARTESIAN_POINT ( 'NONE',  ( -2.117863837641485618E-16, 3.458734125000000326, -0.5124999986344038749 ) ) ;
#2673 = ORIENTED_EDGE ( 'NONE', *, *, #17745, .F. ) ;
#2674 = VECTOR ( 'NONE', #18506, 1000.000000000000000 ) ;
#2675 = FACE_OUTER_BOUND ( 'NONE', #6603, .T. ) ;
#2676 = EDGE_CURVE ( 'NONE', #8667, #10092, #18661, .T. ) ;
#2677 = FACE_OUTER_BOUND ( 'NONE', #20385, .T. ) ;
#2678 = AXIS2_PLACEMENT_3D ( 'NONE', #9265, #20596, #20240 ) ;
#2679 = EDGE_LOOP ( 'NONE', ( #21500, #20742, #17797, #5032 ) ) ;
#2680 = CARTESIAN_POINT ( 'NONE',  ( 34.99999999999999289, 16.40063509461080571, -43.12916512459904794 ) ) ;
#2681 = ORIENTED_EDGE ( 'NONE', *, *, #18759, .F. ) ;
#2682 = CARTESIAN_POINT ( 'NONE',  ( 57.31481816583843170, 12.99999999999999822, 14.93194885905435676 ) ) ;
#2683 = CARTESIAN_POINT ( 'NONE',  ( -69.60000000218495586, 7.499999999999996447, 14.99999999999999645 ) ) ;
#2684 = CARTESIAN_POINT ( 'NONE',  ( 3.458734125000000770, 1.432654583217640498, -2.449999998634404541 ) ) ;
#2685 = CARTESIAN_POINT ( 'NONE',  ( 4.000000000000001776, -1.656854249492379694, 15.43750000000001066 ) ) ;
#2686 = CARTESIAN_POINT ( 'NONE',  ( -1.432654583217639832, -3.458734125000000326, 17.87500000136560274 ) ) ;
#2687 = AXIS2_PLACEMENT_3D ( 'NONE', #14283, #10696, #17975 ) ;
#2688 = CARTESIAN_POINT ( 'NONE',  ( 70.70000000109247651, 7.933012699999995476, 14.14382582708705094 ) ) ;
#2689 = DIRECTION ( 'NONE',  ( 0.000000000000000000, 0.000000000000000000, 1.000000000000000000 ) ) ;
#2690 = VECTOR ( 'NONE', #8286, 1000.000000000000000 ) ;
#2691 = CARTESIAN_POINT ( 'NONE',  ( 57.68981816583843170, 9.931948859054354983, 11.99999999999999645 ) ) ;
#2692 = CARTESIAN_POINT ( 'NONE',  ( -2.445694354108820523, 2.445694354108820523, 5.862500001365596347 ) ) ;
#2693 = CARTESIAN_POINT ( 'NONE',  ( 1.025207404391860050E-15, 3.458734125000000770, 12.43750000136560629 ) ) ;
#2694 = DIRECTION ( 'NONE',  ( -1.000000000000000000, -0.000000000000000000, -0.000000000000000000 ) ) ;
#2695 = CARTESIAN_POINT ( 'NONE',  ( -70.05000000109247082, 7.933012699999995476, 14.99999999999999645 ) ) ;
#2696 = CARTESIAN_POINT ( 'NONE',  ( -70.15000000218495302, 11.03553390593276973, 17.49999999999997158 ) ) ;
#2697 = PLANE ( 'NONE',  #8229 ) ;
#2698 = ORIENTED_EDGE ( 'NONE', *, *, #17416, .T. ) ;
#2699 = B_SPLINE_CURVE_WITH_KNOTS ( 'NONE', 3,
 ( #3230, #8759, #8532, #6961, #14278, #21539 ),
 .UNSPECIFIED., .F., .F.,
 ( 4, 2, 4 ),
 ( -3.640115492410698714E-06, 0.0002066546034006521879, 0.0004169493222937151081 ),
 .UNSPECIFIED. ) ;
#2700 = CARTESIAN_POINT ( 'NONE',  ( 2.828427124746189847, 2.828427124746190291, 3.050000002731189319 ) ) ;
#2701 = VERTEX_POINT ( 'NONE', #12627 ) ;
#2702 = VERTEX_POINT ( 'NONE', #12723 ) ;
#2703 = DIRECTION ( 'NONE',  ( 0.000000000000000000, 0.000000000000000000, 1.000000000000000000 ) ) ;
#2704 = LINE ( 'NONE', #18874, #16750 ) ;
#2705 = VERTEX_POINT ( 'NONE', #14627 ) ;
#2706 = CYLINDRICAL_SURFACE ( 'NONE', #20963, 4.000000000000000000 ) ;
#2707 = VECTOR ( 'NONE', #7921, 1000.000000000000000 ) ;
#2708 = CARTESIAN_POINT ( 'NONE',  ( 67.10000000109248219, 12.06698730000000275, 15.85617417291294196 ) ) ;
#2709 = EDGE_CURVE ( 'NONE', #2825, #7048, #18116, .T. ) ;
#2710 = CARTESIAN_POINT ( 'NONE',  ( 67.05000000109247082, 9.999999999999998224, 12.93301269999999192 ) ) ;
#2711 = EDGE_LOOP ( 'NONE', ( #2739, #10483, #7158, #19964 ) ) ;
#2712 = DIRECTION ( 'NONE',  ( 0.000000000000000000, -0.5877852522924624790, -0.8090169943749551118 ) ) ;
#2713 = CARTESIAN_POINT ( 'NONE',  ( 54.46875000000000000, 5.999999999999987566, 13.34314575050763452 ) ) ;
#2714 = DIRECTION ( 'NONE',  ( 0.3420201433256622736, -0.9396926207859106484, -1.232595164407828100E-31 ) ) ;
#2715 = CARTESIAN_POINT ( 'NONE',  ( -2.445694354108818303, -2.445694354108820523, 17.56250000136560274 ) ) ;
#2716 = VECTOR ( 'NONE', #19508, 1000.000000000000000 ) ;
#2717 = CARTESIAN_POINT ( 'NONE',  ( 72.50000000000000000, 9.999999999999998224, 14.99999999999999645 ) ) ;
#2718 = APPLICATION_CONTEXT ( 'automotive_design' ) ;
#2719 = CARTESIAN_POINT ( 'NONE',  ( 4.999999999999999112, 0.000000000000000000, 0.000000000000000000 ) ) ;
#2720 = ORIENTED_EDGE ( 'NONE', *, *, #16977, .T. ) ;
#2721 = CARTESIAN_POINT ( 'NONE',  ( 60.00000000000000000, 9.999999999999998224, 14.99999999999999645 ) ) ;
#2722 = DIRECTION ( 'NONE',  ( 0.000000000000000000, 0.000000000000000000, -1.000000000000000000 ) ) ;
#2723 = DIRECTION ( 'NONE',  ( 0.000000000000000000, 0.000000000000000000, -1.000000000000000000 ) ) ;
#2724 = EDGE_LOOP ( 'NONE', ( #4740, #22610, #2547, #23003 ) ) ;
#2725 = DIRECTION ( 'NONE',  ( -1.224646799147353207E-16, 0.000000000000000000, -1.000000000000000000 ) ) ;
#2726 = DIRECTION ( 'NONE',  ( -1.000000000000000000, 3.552713678800500929E-15, 0.000000000000000000 ) ) ;
#2727 = CARTESIAN_POINT ( 'NONE',  ( 1.828356344711641102, 3.563200125723180900, -5.433716356636336675E-16 ) ) ;
#2728 = FACE_OUTER_BOUND ( 'NONE', #20664, .T. ) ;
#2729 = VERTEX_POINT ( 'NONE', #5614 ) ;
#2730 = CARTESIAN_POINT ( 'NONE',  ( -6.500000000000000000, 0.000000000000000000, -3.700000000000000178 ) ) ;
#2731 = EDGE_LOOP ( 'NONE', ( #15221, #18067, #14180, #1365 ) ) ;
#2732 = CARTESIAN_POINT ( 'NONE',  ( 4.999999999999999112, 0.000000000000000000, 0.000000000000000000 ) ) ;
#2733 = CARTESIAN_POINT ( 'NONE',  ( 71.15000000218493881, 7.499999999999995559, 16.03553390593273420 ) ) ;
#2734 = ADVANCED_FACE ( 'NONE', ( #335 ), #7669, .T. ) ;
#2735 = DIRECTION ( 'NONE',  ( 7.087422195345011518E-32, 1.000000000000000000, -0.000000000000000000 ) ) ;
#2736 = EDGE_CURVE ( 'NONE', #15611, #13122, #20088, .T. ) ;
#2737 = CARTESIAN_POINT ( 'NONE',  ( 1.600000000000004086, 0.000000000000000000, 0.000000000000000000 ) ) ;
#2738 = CARTESIAN_POINT ( 'NONE',  ( 66.35000000109246798, 11.46158073645647235, 13.53841926354352232 ) ) ;
#2739 = ORIENTED_EDGE ( 'NONE', *, *, #16134, .T. ) ;
#2740 = DIRECTION ( 'NONE',  ( -1.000000000000000000, 0.000000000000000000, -0.000000000000000000 ) ) ;
#2741 = DIRECTION ( 'NONE',  ( -1.000000000000000000, 0.000000000000000000, 0.000000000000000000 ) ) ;
#2742 = ADVANCED_FACE ( 'NONE', ( #1895 ), #9238, .T. ) ;
#2743 = CARTESIAN_POINT ( 'NONE',  ( 69.15000000109246514, 8.538419263543522320, 16.46158073645647235 ) ) ;
#2744 = CARTESIAN_POINT ( 'NONE',  ( -3.458734124999998993, -1.432654583217642497, 14.50000000136560629 ) ) ;
#2745 = DIRECTION ( 'NONE',  ( 0.000000000000000000, 0.000000000000000000, 1.000000000000000000 ) ) ;
#2746 = DIRECTION ( 'NONE',  ( -1.000000000000000000, -0.000000000000000000, -0.000000000000000000 ) ) ;
#2747 = ORIENTED_EDGE ( 'NONE', *, *, #19021, .F. ) ;
#2748 = CARTESIAN_POINT ( 'NONE',  ( -2.465616269789157045, 2.433468530533930974, -3.295601554149322876 ) ) ;
#2749 = CARTESIAN_POINT ( 'NONE',  ( 2.500000000000000000, -2.357898499370432166, 3.035766082959412415E-15 ) ) ;
#2750 = CARTESIAN_POINT ( 'NONE',  ( -3.458734124999998993, -1.432654583217642497, 10.50000000136560452 ) ) ;
#2751 = FACE_OUTER_BOUND ( 'NONE', #19651, .T. ) ;
#2752 = VERTEX_POINT ( 'NONE', #22117 ) ;
#2753 = CARTESIAN_POINT ( 'NONE',  ( 20.00000000000000355, 4.500000000000003553, -2.449293598294706907E-15 ) ) ;
#2754 = ORIENTED_EDGE ( 'NONE', *, *, #11123, .T. ) ;
#2755 = CARTESIAN_POINT ( 'NONE',  ( -68.40000000109246514, 7.933012699999995476, 15.85617417291294196 ) ) ;
#2756 = ORIENTED_EDGE ( 'NONE', *, *, #12561, .F. ) ;
#2757 = CARTESIAN_POINT ( 'NONE',  ( 4.000000000000000000, 1.656854249492381248, -2.012499997268812013 ) ) ;
#2758 = ORIENTED_EDGE ( 'NONE', *, *, #5286, .F. ) ;
#2759 = VERTEX_POINT ( 'NONE', #16522 ) ;
#2760 = CARTESIAN_POINT ( 'NONE',  ( 3.458734125000001658, 1.432654583217640498, 14.25000000136560629 ) ) ;
#2761 = CARTESIAN_POINT ( 'NONE',  ( -4.000000000000000888, 1.656854249492380582, -0.6374999972688124572 ) ) ;
#2762 = ADVANCED_FACE ( 'NONE', ( #11152 ), #15048, .T. ) ;
#2763 = LINE ( 'NONE', #19179, #20522 ) ;
#2764 = ADVANCED_FACE ( 'NONE', ( #7196 ), #2124, .T. ) ;
#2765 = CIRCLE ( 'NONE', #11983, 2.500000000000000444 ) ;
#2766 = CARTESIAN_POINT ( 'NONE',  ( 66.15000000109247935, 11.46158073645647235, 13.53841926354352232 ) ) ;
#2767 = CARTESIAN_POINT ( 'NONE',  ( -70.59999999999999432, 11.76776695296636888, 13.23223304703362579 ) ) ;
#2768 = CARTESIAN_POINT ( 'NONE',  ( -71.50000000000000000, 12.50000000000000000, 14.99999999999999645 ) ) ;
#2769 = ADVANCED_FACE ( 'NONE', ( #5739 ), #13068, .T. ) ;
#2770 = CARTESIAN_POINT ( 'NONE',  ( 53.02893183416157541, 11.17458954617365663, 18.02818770551464311 ) ) ;
#2771 = CARTESIAN_POINT ( 'NONE',  ( 60.00000000000002132, 12.52638886096845816, 13.34932382114196692 ) ) ;
#2772 = ADVANCED_FACE ( 'NONE', ( #19975 ), #5851, .T. ) ;
#2773 = CARTESIAN_POINT ( 'NONE',  ( -3.458734125000000326, -1.432654583217642497, 5.050000001365596347 ) ) ;
#2774 = CARTESIAN_POINT ( 'NONE',  ( 71.54999999999998295, 12.50000000000000000, 16.03553390593273775 ) ) ;
#2775 = CARTESIAN_POINT ( 'NONE',  ( 2.828427124746191179, 2.828427124746190291, 13.75000000273119483 ) ) ;
#2776 = CARTESIAN_POINT ( 'NONE',  ( -2.762848947613220307, 4.746226468750993632, -26.84672628368516811 ) ) ;
#2777 = ORIENTED_EDGE ( 'NONE', *, *, #16217, .T. ) ;
#2778 = CARTESIAN_POINT ( 'NONE',  ( 4.999999999999999112, -9.314797388894882957, -1.239665997526988139 ) ) ;
#2779 = ORIENTED_EDGE ( 'NONE', *, *, #4855, .T. ) ;
#2780 = CARTESIAN_POINT ( 'NONE',  ( 59.40393183416158251, 14.02818770551463956, 13.41119689145323335 ) ) ;
#2781 =( NAMED_UNIT ( * ) PLANE_ANGLE_UNIT ( ) SI_UNIT ( $, .RADIAN. ) );
#2782 = CARTESIAN_POINT ( 'NONE',  ( 3.458734125000000326, 1.432654583217640498, 2.300000001365597679 ) ) ;
#2783 = CARTESIAN_POINT ( 'NONE',  ( 1.432654583217642053, -3.458734124999999437, 0.05000000136559583364 ) ) ;
#2784 = VERTEX_POINT ( 'NONE', #9701 ) ;
#2785 = DIRECTION ( 'NONE',  ( 1.000000000000000000, 0.000000000000000000, 0.000000000000000000 ) ) ;
#2786 = CARTESIAN_POINT ( 'NONE',  ( 72.50000000000000000, 9.999999999999998224, 14.99999999999999645 ) ) ;
#2787 = VECTOR ( 'NONE', #12767, 1000.000000000000000 ) ;
#2788 = VERTEX_POINT ( 'NONE', #4645 ) ;
#2789 = DIRECTION ( 'NONE',  ( 0.3420201433256622736, 0.9396926207859106484, 0.000000000000000000 ) ) ;
#2790 = VERTEX_POINT ( 'NONE', #11743 ) ;
#2791 = CARTESIAN_POINT ( 'NONE',  ( 56.18981816583843170, 9.931948859054354983, 11.99999999999999645 ) ) ;
#2792 = CARTESIAN_POINT ( 'NONE',  ( 5.384454397937118664, 0.000000000000000000, -4.484454397937119197 ) ) ;
#2793 = ADVANCED_FACE ( 'NONE', ( #13422 ), #15339, .T. ) ;
#2794 = PLANE ( 'NONE',  #19024 ) ;
#2795 = CARTESIAN_POINT ( 'NONE',  ( 2.828427124746192067, -2.828427124746189847, 15.37500000000001066 ) ) ;
#2796 = EDGE_CURVE ( 'NONE', #10456, #15720, #20343, .T. ) ;
#2797 = CARTESIAN_POINT ( 'NONE',  ( 66.54999999999999716, 11.03553390593273598, 12.49999999999999289 ) ) ;
#2798 = CARTESIAN_POINT ( 'NONE',  ( 1.971781867644420635E-15, -4.000000000000000000, 13.37500000273119660 ) ) ;
#2799 = CARTESIAN_POINT ( 'NONE',  ( 4.999999999999999112, 0.000000000000000000, 0.000000000000000000 ) ) ;
#2800 = CARTESIAN_POINT ( 'NONE',  ( 69.20000000109246230, 9.143825827087050939, 12.93301269999999370 ) ) ;
#2801 = ADVANCED_FACE ( 'NONE', ( #13648 ), #15423, .T. ) ;
#2802 = CARTESIAN_POINT ( 'NONE',  ( -65.00000000000000000, 15.00000000000000000, 10.00000000000008882 ) ) ;
#2803 = CARTESIAN_POINT ( 'NONE',  ( 54.97106816583843880, 6.971812294485350670, 13.82541045382635403 ) ) ;
#2804 = AXIS2_PLACEMENT_3D ( 'NONE', #12603, #19864, #20442 ) ;
#2805 = CARTESIAN_POINT ( 'NONE',  ( -3.458734125000000770, 0.000000000000000000, 2.987500001365597235 ) ) ;
#2806 = CARTESIAN_POINT ( 'NONE',  ( 1.432654583217641386, 3.458734125000000770, 11.37500000136560452 ) ) ;
#2807 = FILL_AREA_STYLE ('',( #17323 ) ) ;
#2808 = CARTESIAN_POINT ( 'NONE',  ( -70.20000000109246230, 9.143825827087052716, 12.93301269999999192 ) ) ;
#2809 = CARTESIAN_POINT ( 'NONE',  ( 32.96263968033274949, -11.25000000000000355, 5.000000000000079936 ) ) ;
#2810 = FACE_BOUND ( 'NONE', #8956, .T. ) ;
#2811 = ORIENTED_EDGE ( 'NONE', *, *, #3331, .F. ) ;
#2812 = CARTESIAN_POINT ( 'NONE',  ( 4.000000000000000000, -1.942223658245635809, -0.3516579909967643691 ) ) ;
#2813 = FACE_OUTER_BOUND ( 'NONE', #21360, .T. ) ;
#2814 = ORIENTED_EDGE ( 'NONE', *, *, #424, .T. ) ;
#2815 = ORIENTED_EDGE ( 'NONE', *, *, #17717, .T. ) ;
#2816 = CARTESIAN_POINT ( 'NONE',  ( -0.6448876103708541807, -4.246476118072358474, -0.2256878752776773356 ) ) ;
#2817 = AXIS2_PLACEMENT_3D ( 'NONE', #1503, #21609, #1146 ) ;
#2818 = CARTESIAN_POINT ( 'NONE',  ( -66.54999999999999716, 11.03553390593269867, 12.49999999999995559 ) ) ;
#2819 = ORIENTED_EDGE ( 'NONE', *, *, #20584, .F. ) ;
#2820 = PRESENTATION_STYLE_ASSIGNMENT (( #19692 ) ) ;
#2821 = UNCERTAINTY_MEASURE_WITH_UNIT (LENGTH_MEASURE( 1.000000000000000082E-05 ), #14742, 'distance_accuracy_value', 'NONE');
#2822 = CARTESIAN_POINT ( 'NONE',  ( 67.70000000109246230, 10.85617417291294551, 12.93301269999999370 ) ) ;
#2823 = CARTESIAN_POINT ( 'NONE',  ( 69.10000000109246798, 9.143825827087049163, 17.06698729999999742 ) ) ;
#2824 = EDGE_CURVE ( 'NONE', #7050, #8315, #2599, .T. ) ;
#2825 = VERTEX_POINT ( 'NONE', #22609 ) ;
#2826 = FACE_OUTER_BOUND ( 'NONE', #1763, .T. ) ;
#2827 = CARTESIAN_POINT ( 'NONE',  ( 53.53125000000000000, 11.65685424949239923, 18.99999999999998934 ) ) ;
#2828 = CARTESIAN_POINT ( 'NONE',  ( -2.445694354108820523, 2.445694354108820523, 5.612500001365596347 ) ) ;
#2829 = CARTESIAN_POINT ( 'NONE',  ( 67.80000000218494449, 9.999999999999998224, 17.49999999999999645 ) ) ;
#2830 = DIRECTION ( 'NONE',  ( 0.000000000000000000, 0.000000000000000000, -1.000000000000000000 ) ) ;
#2831 = EDGE_LOOP ( 'NONE', ( #2698, #5888, #1244, #23030 ) ) ;
#2832 = LINE ( 'NONE', #6210, #21016 ) ;
#2833 = CYLINDRICAL_SURFACE ( 'NONE', #20097, 4.000000000000001776 ) ;
#2834 = CARTESIAN_POINT ( 'NONE',  ( -13.27237933033274153, -11.25000000000000355, 5.000000000000079936 ) ) ;
#2835 = ORIENTED_EDGE ( 'NONE', *, *, #6728, .F. ) ;
#2836 = CARTESIAN_POINT ( 'NONE',  ( 0.6937372685066666156, -4.453844082567737672, -3.610536846335894445 ) ) ;
#2837 = LINE ( 'NONE', #6576, #23549 ) ;
#2838 = AXIS2_PLACEMENT_3D ( 'NONE', #11973, #13524, #11619 ) ;
#2839 = DIRECTION ( 'NONE',  ( -0.9396926207859107594, -0.3420201433256623291, 1.540743955509804830E-32 ) ) ;
#2840 = ORIENTED_EDGE ( 'NONE', *, *, #174, .T. ) ;
#2841 = DIRECTION ( 'NONE',  ( 0.000000000000000000, 0.000000000000000000, 1.000000000000000000 ) ) ;
#2842 = ORIENTED_EDGE ( 'NONE', *, *, #16566, .F. ) ;
#2843 = CARTESIAN_POINT ( 'NONE',  ( 72.00000000109248788, 10.85617417291294551, 17.06698730000000097 ) ) ;
#2844 = VECTOR ( 'NONE', #17384, 1000.000000000000000 ) ;
#2845 = CIRCLE ( 'NONE', #14351, 7.000000000000000000 ) ;
#2846 = LINE ( 'NONE', #21044, #19902 ) ;
#2847 = CARTESIAN_POINT ( 'NONE',  ( 4.999999999999999112, -1.464956435139619151, 10.90201369670498188 ) ) ;
#2848 = DIRECTION ( 'NONE',  ( -0.000000000000000000, -0.000000000000000000, 1.000000000000000000 ) ) ;
#2849 = CARTESIAN_POINT ( 'NONE',  ( 68.70000000109247651, 10.85617417291294551, 12.93301269999999192 ) ) ;
#2850 = ORIENTED_EDGE ( 'NONE', *, *, #23330, .F. ) ;
#2851 = DIRECTION ( 'NONE',  ( 0.000000000000000000, -1.000000000000000000, -1.047444401652939849E-14 ) ) ;
#2852 = CYLINDRICAL_SURFACE ( 'NONE', #16801, 5.000000000000000888 ) ;
#2853 = CARTESIAN_POINT ( 'NONE',  ( 68.65000000109246514, 9.999999999999998224, 12.93301269999999192 ) ) ;
#2854 = CARTESIAN_POINT ( 'NONE',  ( 3.458734125000001658, 4.235727675282972223E-16, 17.18750000136560629 ) ) ;
#2855 = FACE_OUTER_BOUND ( 'NONE', #14027, .T. ) ;
#2856 = VECTOR ( 'NONE', #23217, 1000.000000000000000 ) ;
#2857 = DIRECTION ( 'NONE',  ( 0.000000000000000000, 0.000000000000000000, 1.000000000000000000 ) ) ;
#2858 = ORIENTED_EDGE ( 'NONE', *, *, #16088, .F. ) ;
#2859 = CARTESIAN_POINT ( 'NONE',  ( -4.000000000000000000, 0.000000000000000000, -0.6999999999999975131 ) ) ;
#2860 = CARTESIAN_POINT ( 'NONE',  ( 4.000000000000000888, 4.898587196589412829E-16, 18.62500000273119483 ) ) ;
#2861 = VECTOR ( 'NONE', #10419, 1000.000000000000114 ) ;
#2862 = DIRECTION ( 'NONE',  ( -0.000000000000000000, -0.000000000000000000, 1.000000000000000000 ) ) ;
#2863 = CARTESIAN_POINT ( 'NONE',  ( -20.00000000000000355, 4.500000000000003553, 2.449293598294706907E-15 ) ) ;
#2864 = ORIENTED_EDGE ( 'NONE', *, *, #6501, .T. ) ;
#2865 = EDGE_CURVE ( 'NONE', #12453, #19131, #1489, .T. ) ;
#2866 = DIRECTION ( 'NONE',  ( 0.3420201433256622736, 0.9396926207859106484, 0.000000000000000000 ) ) ;
#2867 = ORIENTED_EDGE ( 'NONE', *, *, #6589, .F. ) ;
#2868 = CARTESIAN_POINT ( 'NONE',  ( -68.80000000109247082, 12.06698730000000275, 14.14382582708705094 ) ) ;
#2869 = VERTEX_POINT ( 'NONE', #16997 ) ;
#2870 = LINE ( 'NONE', #20948, #21606 ) ;
#2871 = ORIENTED_EDGE ( 'NONE', *, *, #18062, .T. ) ;
#2872 = ORIENTED_EDGE ( 'NONE', *, *, #10537, .F. ) ;
#2873 = CARTESIAN_POINT ( 'NONE',  ( 2.445694354108822299, -2.445694354108820079, 14.06250000136560629 ) ) ;
#2874 = EDGE_CURVE ( 'NONE', #4915, #1949, #16542, .T. ) ;
#2875 = CARTESIAN_POINT ( 'NONE',  ( 5.479999999999998650, 0.000000000000000000, 2.039999999999998259 ) ) ;
#2876 = DIRECTION ( 'NONE',  ( 0.000000000000000000, 0.000000000000000000, 1.000000000000000000 ) ) ;
#2877 = VECTOR ( 'NONE', #4018, 1000.000000000000000 ) ;
#2878 = CARTESIAN_POINT ( 'NONE',  ( 67.20000000109246230, 10.85617417291294551, 17.06698730000000097 ) ) ;
#2879 = CARTESIAN_POINT ( 'NONE',  ( -71.59999999999999432, 11.76776695296636888, 16.76776695296636532 ) ) ;
#2880 = CARTESIAN_POINT ( 'NONE',  ( 0.000000000000000000, 0.000000000000000000, -0.2800830152838844622 ) ) ;
#2881 = CARTESIAN_POINT ( 'NONE',  ( 58.37268183416157541, 7.219692298483935566, 12.12345345202367675 ) ) ;
#2882 = LINE ( 'NONE', #15502, #21512 ) ;
#2883 = CIRCLE ( 'NONE', #5960, 2.500000000000000444 ) ;
#2884 = VECTOR ( 'NONE', #10996, 1000.000000000000000 ) ;
#2885 = CARTESIAN_POINT ( 'NONE',  ( -2.445694354108819635, -2.445694354108820967, 0.1125000013655966247 ) ) ;
#2886 = CARTESIAN_POINT ( 'NONE',  ( 67.05000000218494449, 8.964466094067246260, 17.49999999999999289 ) ) ;
#2887 = DIRECTION ( 'NONE',  ( 0.000000000000000000, -1.000000000000000000, 1.287488025362403787E-15 ) ) ;
#2888 = CARTESIAN_POINT ( 'NONE',  ( -3.999999999999999112, 1.656854249492380804, 11.06250000273119660 ) ) ;
#2889 = FACE_OUTER_BOUND ( 'NONE', #12909, .T. ) ;
#2890 = VERTEX_POINT ( 'NONE', #13771 ) ;
#2891 = EDGE_CURVE ( 'NONE', #21750, #23080, #17322, .T. ) ;
#2892 = ORIENTED_EDGE ( 'NONE', *, *, #8366, .T. ) ;
#2893 = CARTESIAN_POINT ( 'NONE',  ( 54.71643183416158251, 12.97181229448535689, 16.31069182806490758 ) ) ;
#2894 = VECTOR ( 'NONE', #5148, 1000.000000000000000 ) ;
#2895 = B_SPLINE_CURVE_WITH_KNOTS ( 'NONE', 3,
 ( #11448, #7955, #9521, #7483, #14800 ),
 .UNSPECIFIED., .F., .F.,
 ( 4, 1, 4 ),
 ( 0.000000000000000000, 0.002309401076758505356, 0.004618802153517010713 ),
 .UNSPECIFIED. ) ;
#2896 = EDGE_CURVE ( 'NONE', #16753, #13902, #17692, .T. ) ;
#2897 = CARTESIAN_POINT ( 'NONE',  ( 0.5784715375562682338, -3.458734124999999882, 2.012736001390156737 ) ) ;
#2898 = ORIENTED_EDGE ( 'NONE', *, *, #21604, .F. ) ;
#2899 = DIRECTION ( 'NONE',  ( 1.000000000000000000, 0.000000000000000000, 0.000000000000000000 ) ) ;
#2900 = ORIENTED_EDGE ( 'NONE', *, *, #5899, .T. ) ;
#2901 = FACE_OUTER_BOUND ( 'NONE', #23052, .T. ) ;
#2902 = EDGE_LOOP ( 'NONE', ( #16031, #23184 ) ) ;
#2903 = EDGE_CURVE ( 'NONE', #10755, #17794, #3143, .T. ) ;
#2904 = CARTESIAN_POINT ( 'NONE',  ( 58.15856816583844591, 7.028187705514647554, 16.31069182806492179 ) ) ;
#2905 = CARTESIAN_POINT ( 'NONE',  ( -66.85000000218495586, 12.50000000000000000, 16.03553390593273420 ) ) ;
#2906 = CARTESIAN_POINT ( 'NONE',  ( -2.117863837641485618E-16, 3.458734125000000770, -1.262499998634402765 ) ) ;
#2907 = FACE_OUTER_BOUND ( 'NONE', #13297, .T. ) ;
#2908 = CARTESIAN_POINT ( 'NONE',  ( 3.458734125000001658, 1.432654583217640498, 18.25000000136560629 ) ) ;
#2909 = CARTESIAN_POINT ( 'NONE',  ( 9.920644283265380691E-16, 4.000000000000000000, 13.87500000273119483 ) ) ;
#2910 = CARTESIAN_POINT ( 'NONE',  ( 56.34375000000000711, 8.757359312880723223, 18.00000000000000355 ) ) ;
#2911 = CARTESIAN_POINT ( 'NONE',  ( 68.80000000109247082, 10.85617417291294551, 17.06698729999999742 ) ) ;
#2912 = CARTESIAN_POINT ( 'NONE',  ( -20.00000000000001066, 4.500000000000003553, -50.00000000000000000 ) ) ;
#2913 = CARTESIAN_POINT ( 'NONE',  ( 51.68981816583844591, 9.931948859054354983, 11.99999999999999645 ) ) ;
#2914 = EDGE_CURVE ( 'NONE', #6569, #13807, #4525, .T. ) ;
#2915 = CARTESIAN_POINT ( 'NONE',  ( -1.432654583217641164, -3.458734125000000326, 0.1750000013655959585 ) ) ;
#2916 = CARTESIAN_POINT ( 'NONE',  ( -1.432654583217639166, 3.458734125000000770, 10.50000000136560629 ) ) ;
#2917 = CYLINDRICAL_SURFACE ( 'NONE', #17603, 11.00000000000000000 ) ;
#2918 = CARTESIAN_POINT ( 'NONE',  ( -69.35000000109246798, 8.538419263543524096, 13.53841926354352054 ) ) ;
#2919 = VERTEX_POINT ( 'NONE', #6088 ) ;
#2920 = CARTESIAN_POINT ( 'NONE',  ( 4.024499207728657879, -2.323545700935587988, -3.572172305156509964 ) ) ;
#2921 = CARTESIAN_POINT ( 'NONE',  ( -2.828427124746190291, 2.828427124746190291, -1.824999999999998401 ) ) ;
#2922 = ORIENTED_EDGE ( 'NONE', *, *, #11454, .F. ) ;
#2923 = CARTESIAN_POINT ( 'NONE',  ( 4.714285714285714413, 0.000000000000000000, 2.039999999999998259 ) ) ;
#2924 = CARTESIAN_POINT ( 'NONE',  ( 2.828427124746189847, 2.828427124746190291, -0.9499999972688126793 ) ) ;
#2925 = EDGE_CURVE ( 'NONE', #3058, #2194, #5833, .T. ) ;
#2926 = VERTEX_POINT ( 'NONE', #17352 ) ;
#2927 = EDGE_LOOP ( 'NONE', ( #23459, #5244, #12916, #5062 ) ) ;
#2928 = CARTESIAN_POINT ( 'NONE',  ( -1.312671235360383548, -3.860931062424228788, -0.05923475698271369466 ) ) ;
#2929 = VECTOR ( 'NONE', #5199, 1000.000000000000114 ) ;
#2930 = CARTESIAN_POINT ( 'NONE',  ( 0.000000000000000000, 9.241976615262160522, -1.699438267350405818 ) ) ;
#2931 = ORIENTED_EDGE ( 'NONE', *, *, #5867, .T. ) ;
#2932 = EDGE_CURVE ( 'NONE', #16281, #14518, #8255, .T. ) ;
#2933 = CARTESIAN_POINT ( 'NONE',  ( -16.41397198033274307, -11.25000000000000355, 5.000000000000079936 ) ) ;
#2934 = EDGE_CURVE ( 'NONE', #10781, #21477, #15575, .T. ) ;
#2935 = CARTESIAN_POINT ( 'NONE',  ( 66.80000000109247082, 9.143825827087050939, 12.93301269999999370 ) ) ;
#2936 = VECTOR ( 'NONE', #23113, 1000.000000000000000 ) ;
#2937 = CARTESIAN_POINT ( 'NONE',  ( 66.70000000109246230, 9.143825827087049163, 17.06698729999999742 ) ) ;
#2938 = DIRECTION ( 'NONE',  ( 0.000000000000000000, 0.000000000000000000, 1.000000000000000000 ) ) ;
#2939 = DIRECTION ( 'NONE',  ( -1.000000000000000000, 0.000000000000000000, 0.000000000000000000 ) ) ;
#2940 = CARTESIAN_POINT ( 'NONE',  ( 53.81250000000000711, 14.00000000000000000, 14.99999999999997691 ) ) ;
#2941 = CARTESIAN_POINT ( 'NONE',  ( -2.445694354108820523, 2.445694354108820523, 4.612500001365595459 ) ) ;
#2942 = CARTESIAN_POINT ( 'NONE',  ( -1.432654583217638944, 3.458734125000000326, 13.25000000136560274 ) ) ;
#2943 = CARTESIAN_POINT ( 'NONE',  ( 0.000000000000000000, 9.241976615262160522, -1.699438267350405818 ) ) ;
#2944 = AXIS2_PLACEMENT_3D ( 'NONE', #21848, #14587, #7620 ) ;
#2945 = CARTESIAN_POINT ( 'NONE',  ( 4.999999999999999112, 0.000000000000000000, 0.000000000000000000 ) ) ;
#2946 = ORIENTED_EDGE ( 'NONE', *, *, #13820, .F. ) ;
#2947 = CARTESIAN_POINT ( 'NONE',  ( -8.696997796766190447, -9.000000000000005329, 10.00000000000008882 ) ) ;
#2948 = CARTESIAN_POINT ( 'NONE',  ( -1.799999999999996048, 1.102182119232620672E-15, 9.000000000000021316 ) ) ;
#2949 = CARTESIAN_POINT ( 'NONE',  ( -66.90000000000000568, 9.999999999999998224, 17.49999999999999645 ) ) ;
#2950 = VECTOR ( 'NONE', #12805, 1000.000000000000000 ) ;
#2951 = AXIS2_PLACEMENT_3D ( 'NONE', #15519, #11934, #15637 ) ;
#2952 = ORIENTED_EDGE ( 'NONE', *, *, #15835, .F. ) ;
#2953 = CARTESIAN_POINT ( 'NONE',  ( -3.999999999999999112, 0.000000000000000000, 14.12500000273119660 ) ) ;
#2954 = FACE_OUTER_BOUND ( 'NONE', #12220, .T. ) ;
#2955 = ADVANCED_FACE ( 'NONE', ( #21031 ), #19245, .F. ) ;
#2956 = DIRECTION ( 'NONE',  ( 0.000000000000000000, 0.000000000000000000, -1.000000000000000000 ) ) ;
#2957 = VERTEX_POINT ( 'NONE', #1039 ) ;
#2958 = CARTESIAN_POINT ( 'NONE',  ( 65.80000000218494449, 9.999999999999998224, 12.49999999999999289 ) ) ;
#2959 = EDGE_LOOP ( 'NONE', ( #76, #17152, #20067, #4280 ) ) ;
#2960 = EDGE_CURVE ( 'NONE', #10612, #14572, #19583, .T. ) ;
#2961 = DIRECTION ( 'NONE',  ( 0.000000000000000000, -0.000000000000000000, -1.000000000000000000 ) ) ;
#2962 = CARTESIAN_POINT ( 'NONE',  ( 69.95000000218493597, 12.50000000000000000, 13.96446609406725869 ) ) ;
#2963 = VECTOR ( 'NONE', #21400, 1000.000000000000000 ) ;
#2964 = CARTESIAN_POINT ( 'NONE',  ( 50.00000000000000000, 10.00000000000001599, 34.11836509645782201 ) ) ;
#2965 = CARTESIAN_POINT ( 'NONE',  ( 4.000000000000000888, 1.656854249492381248, 11.56250000000001066 ) ) ;
#2966 = CARTESIAN_POINT ( 'NONE',  ( 66.90000000109247935, 7.933012699999995476, 14.14382582708705094 ) ) ;
#2967 = VERTEX_POINT ( 'NONE', #10539 ) ;
#2968 = B_SPLINE_CURVE_WITH_KNOTS ( 'NONE', 1,
 ( #8693, #17902 ),
 .UNSPECIFIED., .F., .F.,
 ( 2, 2 ),
 ( 0.000000000000000000, 1.000000000000000000 ),
 .UNSPECIFIED. ) ;
#2969 = AXIS2_PLACEMENT_3D ( 'NONE', #9767, #13600, #22670 ) ;
#2970 = DIRECTION ( 'NONE',  ( -1.224646799147353207E-16, 0.000000000000000000, -1.000000000000000000 ) ) ;
#2971 = DIRECTION ( 'NONE',  ( 4.625929269271486900E-16, -1.000000000000000000, -5.665129472695380173E-32 ) ) ;
#2972 = CARTESIAN_POINT ( 'NONE',  ( 69.95000000109247651, 8.538419263543522320, 16.46158073645647235 ) ) ;
#2973 = CARTESIAN_POINT ( 'NONE',  ( 1.432654583217641164, 3.458734125000000326, 11.12500000136560452 ) ) ;
#2974 = DIRECTION ( 'NONE',  ( 1.224646799147353207E-16, -0.000000000000000000, 1.000000000000000000 ) ) ;
#2975 = CARTESIAN_POINT ( 'NONE',  ( 6.499999999999999112, 0.000000000000000000, 1.734723475976807094E-15 ) ) ;
#2976 = ORIENTED_EDGE ( 'NONE', *, *, #19049, .T. ) ;
#2977 = CARTESIAN_POINT ( 'NONE',  ( -4.000000000000000000, 0.000000000000000000, -2.699999999999999289 ) ) ;
#2978 = DIRECTION ( 'NONE',  ( -1.000000000000000000, 0.000000000000000000, 0.000000000000000000 ) ) ;
#2979 = CARTESIAN_POINT ( 'NONE',  ( 66.65000000000000568, 12.50000000000000000, 13.96446609406725692 ) ) ;
#2980 = CARTESIAN_POINT ( 'NONE',  ( -2.000000000000007550, -3.464101615137749945, 0.000000000000000000 ) ) ;
#2981 = ORIENTED_EDGE ( 'NONE', *, *, #3861, .T. ) ;
#2982 = PRESENTATION_LAYER_ASSIGNMENT (  '', '', ( #2212 ) ) ;
#2983 = CARTESIAN_POINT ( 'NONE',  ( -0.8800590352214046064, 5.420839058164813373, 10.00000000000000888 ) ) ;
#2984 = VERTEX_POINT ( 'NONE', #8497 ) ;
#2985 = CARTESIAN_POINT ( 'NONE',  ( -68.60000000109246798, 9.143825827087050939, 12.93301269999999370 ) ) ;
#2986 = ITEM_DEFINED_TRANSFORMATION ( 'NONE', 'NONE', #8410,  #7318 ) ;
#2987 =( BOUNDED_CURVE ( )  B_SPLINE_CURVE ( 2, ( #6364, #6484, #4558, #21173, #19164, #720, #6124, #13452, #4672 ),
 .UNSPECIFIED., .F., .F. ) 
 B_SPLINE_CURVE_WITH_KNOTS ( ( 3, 2, 2, 2, 3 ),
 ( 0.6999999999999999556, 0.7125000000000000222, 0.7249999999999999778, 0.7375000000000000444, 0.7500000000000000000 ),
 .UNSPECIFIED. ) 
 CURVE ( )  GEOMETRIC_REPRESENTATION_ITEM ( )  RATIONAL_B_SPLINE_CURVE ( ( 1.000000000000000000, 0.9238795325112867385, 1.000000000000000000, 0.9238795325112867385, 1.000000000000000000, 0.9238795325112867385, 1.000000000000000000, 0.9238795325112867385, 1.000000000000000000 ) ) 
 REPRESENTATION_ITEM ( '' )  );
#2988 = ORIENTED_EDGE ( 'NONE', *, *, #5991, .T. ) ;
#2989 = FACE_OUTER_BOUND ( 'NONE', #6826, .T. ) ;
#2990 = VERTEX_POINT ( 'NONE', #17473 ) ;
#2991 = AXIS2_PLACEMENT_3D ( 'NONE', #16723, #301, #7638 ) ;
#2992 = VERTEX_POINT ( 'NONE', #3313 ) ;
#2993 = CARTESIAN_POINT ( 'NONE',  ( -3.458734124999999437, 1.432654583217640498, 14.62500000136560629 ) ) ;
#2994 = CARTESIAN_POINT ( 'NONE',  ( 4.000000000000000000, 1.656854249492381248, -1.012499997268812901 ) ) ;
#2995 = CARTESIAN_POINT ( 'NONE',  ( -66.75000000218494733, 12.50000000000000000, 13.96446609406725692 ) ) ;
#2996 = PRODUCT_DEFINITION ( 'UNKNOWN', '', #17578, #4530 ) ;
#2997 = CYLINDRICAL_SURFACE ( 'NONE', #18292, 4.000000000000000000 ) ;
#2998 = VECTOR ( 'NONE', #12138, 1000.000000000000000 ) ;
#2999 = CIRCLE ( 'NONE', #8002, 5.000000000000004441 ) ;
#3000 = EDGE_CURVE ( 'NONE', #2788, #20225, #15910, .T. ) ;
#3001 = CARTESIAN_POINT ( 'NONE',  ( -69.29999999999999716, 9.999999999999998224, 17.49999999999999645 ) ) ;
#3002 = LINE ( 'NONE', #23479, #20974 ) ;
#3003 = CARTESIAN_POINT ( 'NONE',  ( 60.00000000000005684, 13.02863400130356375, 14.80978507604997851 ) ) ;
#3004 = CIRCLE ( 'NONE', #19068, 4.999999999999999112 ) ;
#3005 = CARTESIAN_POINT ( 'NONE',  ( -2.445694354108819635, -2.445694354108820967, -1.887499998634403431 ) ) ;
#3006 = DIRECTION ( 'NONE',  ( -1.000000000000000000, -0.000000000000000000, -0.000000000000000000 ) ) ;
#3007 = CYLINDRICAL_SURFACE ( 'NONE', #23424, 2.500000000000002220 ) ;
#3008 = CARTESIAN_POINT ( 'NONE',  ( 3.458734125000001214, 4.235727675282971730E-16, 15.93750000136560629 ) ) ;
#3009 = CARTESIAN_POINT ( 'NONE',  ( 4.999999999999999112, -9.915734732513254102, 4.762163868918236176 ) ) ;
#3010 = ORIENTED_EDGE ( 'NONE', *, *, #8593, .F. ) ;
#3011 = CARTESIAN_POINT ( 'NONE',  ( -1.520000000000000462, 1.010590785124388747E-15, 8.239200000000002078 ) ) ;
#3012 = VERTEX_POINT ( 'NONE', #2949 ) ;
#3013 = CARTESIAN_POINT ( 'NONE',  ( 54.81018183416157541, 12.99999999999999822, 15.06805114094562192 ) ) ;
#3014 = CARTESIAN_POINT ( 'NONE',  ( -70.35000000109248219, 11.46158073645647235, 16.46158073645647235 ) ) ;
#3015 =( NAMED_UNIT ( * ) SI_UNIT ( $, .STERADIAN. ) SOLID_ANGLE_UNIT ( ) );
#3016 = AXIS2_PLACEMENT_3D ( 'NONE', #5876, #11407, #18684 ) ;
#3017 = DIRECTION ( 'NONE',  ( 0.000000000000000000, 0.000000000000000000, -1.000000000000000000 ) ) ;
#3018 = ORIENTED_EDGE ( 'NONE', *, *, #14669, .F. ) ;
#3019 = LINE ( 'NONE', #23137, #19415 ) ;
#3020 = AXIS2_PLACEMENT_3D ( 'NONE', #3457, #10794, #8993 ) ;
#3021 = ORIENTED_EDGE ( 'NONE', *, *, #18793, .F. ) ;
#3022 = DIRECTION ( 'NONE',  ( -1.000000000000000000, 0.000000000000000000, 1.982541115402065110E-16 ) ) ;
#3023 = ORIENTED_EDGE ( 'NONE', *, *, #17689, .T. ) ;
#3024 = CARTESIAN_POINT ( 'NONE',  ( 59.00231816583843170, 12.07320092032949610, 12.83056023321021044 ) ) ;
#3025 =( BOUNDED_CURVE ( )  B_SPLINE_CURVE ( 2, ( #8882, #8751, #14270, #21532, #3343, #1541, #10685, #17961, #16175 ),
 .UNSPECIFIED., .F., .F. ) 
 B_SPLINE_CURVE_WITH_KNOTS ( ( 3, 2, 2, 2, 3 ),
 ( 0.8000000000000000444, 0.8125000000000000000, 0.8249999999999999556, 0.8375000000000000222, 0.8499999999999999778 ),
 .UNSPECIFIED. ) 
 CURVE ( )  GEOMETRIC_REPRESENTATION_ITEM ( )  RATIONAL_B_SPLINE_CURVE ( ( 1.000000000000000000, 0.9238795325112867385, 1.000000000000000000, 0.9238795325112867385, 1.000000000000000000, 0.9238795325112867385, 1.000000000000000000, 0.9238795325112867385, 1.000000000000000000 ) ) 
 REPRESENTATION_ITEM ( '' )  );
#3026 = MECHANICAL_DESIGN_GEOMETRIC_PRESENTATION_REPRESENTATION (  '', ( #8030 ), #3797 ) ;
#3027 = CARTESIAN_POINT ( 'NONE',  ( -65.95000000218495018, 12.50000000000000000, 13.96446609406725869 ) ) ;
#3028 = AXIS2_PLACEMENT_3D ( 'NONE', #10356, #6621, #12268 ) ;
#3029 = DIRECTION ( 'NONE',  ( 0.000000000000000000, -0.5877852522924625900, -0.8090169943749552228 ) ) ;
#3030 = APPLICATION_CONTEXT ( 'automotive_design' ) ;
#3031 = ADVANCED_FACE ( 'NONE', ( #21622 ), #8524, .T. ) ;
#3032 = DIRECTION ( 'NONE',  ( -1.000000000000000000, -4.625929269271486900E-16, 1.224646799147353207E-16 ) ) ;
#3033 = CARTESIAN_POINT ( 'NONE',  ( 2.445694354108822299, -2.445694354108820079, 15.06250000136560452 ) ) ;
#3034 = EDGE_CURVE ( 'NONE', #11666, #22477, #2765, .T. ) ;
#3035 = CARTESIAN_POINT ( 'NONE',  ( 1.656854249492384135, -3.999999999999999112, 15.43750000273119660 ) ) ;
#3036 = CIRCLE ( 'NONE', #11862, 8.239200000000002078 ) ;
#3037 = CARTESIAN_POINT ( 'NONE',  ( 66.99999999999998579, 8.232233047033627571, 16.76776695296636532 ) ) ;
#3038 = CIRCLE ( 'NONE', #22548, 8.749000000000002331 ) ;
#3039 = FACE_OUTER_BOUND ( 'NONE', #663, .T. ) ;
#3040 = CARTESIAN_POINT ( 'NONE',  ( 59.34375000000000711, 8.757359312880723223, 18.00000000000000355 ) ) ;
#3041 = CARTESIAN_POINT ( 'NONE',  ( -3.458734125000000770, 0.000000000000000000, 0.9875000013655956810 ) ) ;
#3042 = CARTESIAN_POINT ( 'NONE',  ( 1.432654583217643163, -3.458734124999999882, 12.00000000136560452 ) ) ;
#3043 = EDGE_CURVE ( 'NONE', #9561, #17175, #8918, .T. ) ;
#3044 = CARTESIAN_POINT ( 'NONE',  ( -6.123233995736766085E-15, 0.000000000000000000, -50.00000000000000000 ) ) ;
#3045 = CARTESIAN_POINT ( 'NONE',  ( -69.80000000109247082, 10.85617417291294551, 17.06698730000000097 ) ) ;
#3046 = EDGE_LOOP ( 'NONE', ( #15090, #17739, #20445, #10941, #8859, #7784 ) ) ;
#3047 = CARTESIAN_POINT ( 'NONE',  ( 0.1221691407165617638, -8.974600000000002353, 5.000000000000079936 ) ) ;
#3048 = DIRECTION ( 'NONE',  ( 1.224646799147353207E-16, -0.000000000000000000, 1.000000000000000000 ) ) ;
#3049 = ORIENTED_EDGE ( 'NONE', *, *, #10074, .F. ) ;
#3050 = FACE_OUTER_BOUND ( 'NONE', #6832, .T. ) ;
#3052 = VECTOR ( 'NONE', #20998, 1000.000000000000000 ) ;
#3051 =( NAMED_UNIT ( * ) SI_UNIT ( $, .STERADIAN. ) SOLID_ANGLE_UNIT ( ) );
#3053 = CARTESIAN_POINT ( 'NONE',  ( 2.828427124746189847, 2.828427124746190291, 2.050000002731188431 ) ) ;
#3054 = ORIENTED_EDGE ( 'NONE', *, *, #6171, .F. ) ;
#3055 = ORIENTED_EDGE ( 'NONE', *, *, #18040, .T. ) ;
#3056 = PLANE ( 'NONE',  #18656 ) ;
#3057 = CARTESIAN_POINT ( 'NONE',  ( 0.000000000000000000, 0.000000000000000000, 20.00000000000001066 ) ) ;
#3058 = VERTEX_POINT ( 'NONE', #13887 ) ;
#3059 = CARTESIAN_POINT ( 'NONE',  ( 1.519999999999999352, 6.760799999999997034, 0.000000000000000000 ) ) ;
#3060 = CIRCLE ( 'NONE', #9211, 2.500000000000000444 ) ;
#3061 = AXIS2_PLACEMENT_3D ( 'NONE', #19098, #8899, #20874 ) ;
#3062 = UNCERTAINTY_MEASURE_WITH_UNIT (LENGTH_MEASURE( 1.000000000000000082E-05 ), #21533, 'distance_accuracy_value', 'NONE');
#3063 = CARTESIAN_POINT ( 'NONE',  ( -1.656854249492379250, 4.000000000000000000, 11.81250000000001066 ) ) ;
#3064 = EDGE_CURVE ( 'NONE', #21915, #22477, #1268, .T. ) ;
#3065 = DIRECTION ( 'NONE',  ( 1.000000000000000000, 0.000000000000000000, 0.000000000000000000 ) ) ;
#3066 = VECTOR ( 'NONE', #6423, 1000.000000000000000 ) ;
#3067 = VECTOR ( 'NONE', #19537, 1000.000000000000000 ) ;
#3068 = CARTESIAN_POINT ( 'NONE',  ( 67.45000000109246230, 9.999999999999998224, 17.06698730000000097 ) ) ;
#3069 = EDGE_CURVE ( 'NONE', #16674, #18227, #4758, .T. ) ;
#3070 = CARTESIAN_POINT ( 'NONE',  ( -65.80000000218494449, 9.999999999999998224, 12.49999999999999289 ) ) ;
#3071 = CARTESIAN_POINT ( 'NONE',  ( -15.00000000000001066, -10.00000000000000000, -49.99999999999999289 ) ) ;
#3072 = CARTESIAN_POINT ( 'NONE',  ( 56.47106816583845301, 5.971812294485345340, 13.41119689145326710 ) ) ;
#3073 = CARTESIAN_POINT ( 'NONE',  ( 3.458734125000000326, 1.432654583217640498, 4.300000001365595459 ) ) ;
#3074 = EDGE_CURVE ( 'NONE', #12101, #18107, #850, .T. ) ;
#3075 = CARTESIAN_POINT ( 'NONE',  ( 3.458734125000001214, 1.432654583217640498, 16.00000000136560629 ) ) ;
#3076 = FACE_OUTER_BOUND ( 'NONE', #18732, .T. ) ;
#3077 = ADVANCED_FACE ( 'NONE', ( #1515, #3192 ), #12094, .T. ) ;
#3078 = DIRECTION ( 'NONE',  ( 0.000000000000000000, 0.000000000000000000, 1.000000000000000000 ) ) ;
#3079 = ORIENTED_EDGE ( 'NONE', *, *, #3194, .F. ) ;
#3080 = CARTESIAN_POINT ( 'NONE',  ( -3.502865032392102673, 0.9776794494524829737, 2.039999999999989821 ) ) ;
#3081 = CARTESIAN_POINT ( 'NONE',  ( 40.13469571966727045, -11.25000000000000355, 5.000000000000079936 ) ) ;
#3082 = CARTESIAN_POINT ( 'NONE',  ( -4.000000000000000000, -1.656854249492383024, -1.637499999999997957 ) ) ;
#3083 = VECTOR ( 'NONE', #13544, 1000.000000000000000 ) ;
#3084 = VERTEX_POINT ( 'NONE', #14359 ) ;
#3085 = CARTESIAN_POINT ( 'NONE',  ( 60.00000000000000711, 15.00000000000000000, 10.00000000000007105 ) ) ;
#3086 = CARTESIAN_POINT ( 'NONE',  ( -67.64999999999999147, 11.03553390593272887, 17.50000000000001066 ) ) ;
#3087 = CARTESIAN_POINT ( 'NONE',  ( 59.81250000000000711, 14.00000000000000000, 14.99999999999997691 ) ) ;
#3088 = ORIENTED_EDGE ( 'NONE', *, *, #20465, .T. ) ;
#3089 = DIRECTION ( 'NONE',  ( -1.000000000000000000, 0.000000000000000000, 0.000000000000000000 ) ) ;
#3090 = ORIENTED_EDGE ( 'NONE', *, *, #3478, .T. ) ;
#3091 = CARTESIAN_POINT ( 'NONE',  ( 54.93750000000000711, 10.00000000000001776, 18.99999999999999645 ) ) ;
#3092 = CARTESIAN_POINT ( 'NONE',  ( 67.70000000218493597, 11.76776695296636888, 16.76776695296636532 ) ) ;
#3093 = DIRECTION ( 'NONE',  ( -1.000000000000000000, -0.000000000000000000, -0.000000000000000000 ) ) ;
#3094 = CARTESIAN_POINT ( 'NONE',  ( -0.6666666666666666297, -4.233901974057276973, -3.300726591567087365 ) ) ;
#3095 = EDGE_CURVE ( 'NONE', #402, #9354, #10182, .T. ) ;
#3096 = CARTESIAN_POINT ( 'NONE',  ( 67.45000000109246230, 9.999999999999998224, 17.06698730000000097 ) ) ;
#3097 = ORIENTED_EDGE ( 'NONE', *, *, #18520, .F. ) ;
#3098 = DIRECTION ( 'NONE',  ( 1.000000000000000000, 0.000000000000000000, 0.000000000000000000 ) ) ;
#3099 = EDGE_CURVE ( 'NONE', #11761, #20113, #20430, .T. ) ;
#3100 = DIRECTION ( 'NONE',  ( -1.000000000000000000, -0.000000000000000000, 0.000000000000000000 ) ) ;
#3101 = EDGE_CURVE ( 'NONE', #17422, #16065, #23187, .T. ) ;
#3102 = CARTESIAN_POINT ( 'NONE',  ( 68.15000000109246514, 11.46158073645647235, 16.46158073645647235 ) ) ;
#3103 = CARTESIAN_POINT ( 'NONE',  ( 3.458734125000001658, 1.432654583217640498, 18.25000000136560629 ) ) ;
#3104 = CARTESIAN_POINT ( 'NONE',  ( -1.600000000000004086, 9.887492094615969966E-16, 8.073750000000021743 ) ) ;
#3105 = EDGE_CURVE ( 'NONE', #1597, #15665, #23422, .T. ) ;
#3106 = DIRECTION ( 'NONE',  ( 0.000000000000000000, 0.000000000000000000, 1.000000000000000000 ) ) ;
#3107 = ORIENTED_EDGE ( 'NONE', *, *, #19599, .F. ) ;
#3108 = CARTESIAN_POINT ( 'NONE',  ( -2.449293598294706907E-16, 4.000000000000000000, -0.9499999999999977351 ) ) ;
#3109 = CARTESIAN_POINT ( 'NONE',  ( 59.15625000000001421, 7.000000000000002665, 16.24264068711929099 ) ) ;
#3110 = DIRECTION ( 'NONE',  ( 0.000000000000000000, 0.000000000000000000, -1.000000000000000000 ) ) ;
#3111 = CARTESIAN_POINT ( 'NONE',  ( 0.000000000000000000, 0.000000000000000000, 0.000000000000000000 ) ) ;
#3112 = B_SPLINE_CURVE_WITH_KNOTS ( 'NONE', 3,
 ( #3548, #18396, #13035, #16374, #10995, #5465 ),
 .UNSPECIFIED., .F., .F.,
 ( 4, 2, 4 ),
 ( 0.006695446894088489739, 0.008593684019695166376, 0.01049192114530184475 ),
 .UNSPECIFIED. ) ;
#3113 = ORIENTED_EDGE ( 'NONE', *, *, #2319, .F. ) ;
#3114 = DIRECTION ( 'NONE',  ( 0.000000000000000000, 0.000000000000000000, 1.000000000000000000 ) ) ;
#3115 = CARTESIAN_POINT ( 'NONE',  ( 3.680118525130245732, -2.494084732383344605, -0.3507732604232533524 ) ) ;
#3116 = ORIENTED_EDGE ( 'NONE', *, *, #18915, .F. ) ;
#3117 = CARTESIAN_POINT ( 'NONE',  ( -65.85000000218495586, 11.03553390593269867, 12.49999999999995559 ) ) ;
#3118 = ORIENTED_EDGE ( 'NONE', *, *, #10409, .F. ) ;
#3119 = CARTESIAN_POINT ( 'NONE',  ( -4.898587196589412829E-16, 0.000000000000000000, -4.000000000000000000 ) ) ;
#3120 = EDGE_LOOP ( 'NONE', ( #8165, #22127, #18181, #17207 ) ) ;
#3121 = CARTESIAN_POINT ( 'NONE',  ( 2.445694354108822299, -2.445694354108820079, 11.06250000136560452 ) ) ;
#3122 = CARTESIAN_POINT ( 'NONE',  ( 0.1221691407165617638, -8.974600000000002353, 10.00000000000008882 ) ) ;
#3123 = CARTESIAN_POINT ( 'NONE',  ( -67.90000000218495302, 8.232233047033627571, 16.76776695296636532 ) ) ;
#3124 = CARTESIAN_POINT ( 'NONE',  ( 0.000000000000000000, -8.475820894093002877, 4.057423117305363647 ) ) ;
#3125 = LINE ( 'NONE', #18092, #9851 ) ;
#3126 = CARTESIAN_POINT ( 'NONE',  ( -71.29999999999998295, 9.999999999999998224, 12.49999999999999289 ) ) ;
#3127 = CARTESIAN_POINT ( 'NONE',  ( -2.682243648011671588, -3.070208061305317759, -0.04852650426602272971 ) ) ;
#3128 = ADVANCED_FACE ( 'NONE', ( #1383 ), #16030, .F. ) ;
#3129 = CARTESIAN_POINT ( 'NONE',  ( 28.38725814676620018, -9.000000000000007105, 10.00000000000008882 ) ) ;
#3130 =( BOUNDED_CURVE ( )  B_SPLINE_CURVE ( 2, ( #5109, #16145, #7039, #14355, #21618, #19827, #8970, #16261, #9672 ),
 .UNSPECIFIED., .F., .F. ) 
 B_SPLINE_CURVE_WITH_KNOTS ( ( 3, 2, 2, 2, 3 ),
 ( 0.1875000000000010270, 0.2031250000000009437, 0.2187500000000008327, 0.2343750000000007494, 0.2500000000000006661 ),
 .UNSPECIFIED. ) 
 CURVE ( )  GEOMETRIC_REPRESENTATION_ITEM ( )  RATIONAL_B_SPLINE_CURVE ( ( 0.9999999999999950040, 0.9238795325112917345, 1.000000000000000000, 0.9238795325112867385, 1.000000000000000000, 0.9238795325112867385, 1.000000000000000000, 0.9238795325112835188, 1.000000000000003331 ) ) 
 REPRESENTATION_ITEM ( '' )  );
#3131 = CARTESIAN_POINT ( 'NONE',  ( 1.432654583217640276, 3.458734125000000770, -1.324999998634403653 ) ) ;
#3132 = CARTESIAN_POINT ( 'NONE',  ( 45.00000000000000000, -9.796556200126357083, 11.00000000000008882 ) ) ;
#3133 = CARTESIAN_POINT ( 'NONE',  ( 3.458734125000001214, 4.235727675282971730E-16, 18.93750000136560629 ) ) ;
#3134 = ORIENTED_EDGE ( 'NONE', *, *, #1290, .T. ) ;
#3135 = CARTESIAN_POINT ( 'NONE',  ( 0.000000000000000000, 7.593217523260696211, -7.958834565716683684 ) ) ;
#3136 = ORIENTED_EDGE ( 'NONE', *, *, #18444, .F. ) ;
#3137 = CARTESIAN_POINT ( 'NONE',  ( 60.90393183416158962, 14.02818770551463956, 13.41119689145323335 ) ) ;
#3138 = CARTESIAN_POINT ( 'NONE',  ( -67.15000000109247935, 11.46158073645647235, 16.46158073645647235 ) ) ;
#3139 = CYLINDRICAL_SURFACE ( 'NONE', #17820, 2.500000000000002220 ) ;
#3140 = VERTEX_POINT ( 'NONE', #5822 ) ;
#3141 = DIRECTION ( 'NONE',  ( 1.000000000000000000, 0.000000000000000000, 0.000000000000000000 ) ) ;
#3142 = ORIENTED_EDGE ( 'NONE', *, *, #12124, .F. ) ;
#3143 = CIRCLE ( 'NONE', #8147, 11.00000000000000000 ) ;
#3144 = DIRECTION ( 'NONE',  ( 0.000000000000000000, 0.000000000000000000, 1.000000000000000000 ) ) ;
#3145 = EDGE_LOOP ( 'NONE', ( #7836, #14584, #6555, #11805 ) ) ;
#3146 = CARTESIAN_POINT ( 'NONE',  ( 54.78356816583844591, 8.689308171935074654, 12.02818770551464489 ) ) ;
#3147 = CARTESIAN_POINT ( 'NONE',  ( -68.90000000218495302, 8.232233047033629347, 13.23223304703362402 ) ) ;
#3148 = LINE ( 'NONE', #10492, #20905 ) ;
#3149 = CARTESIAN_POINT ( 'NONE',  ( 45.00000000000000000, -10.00000000000001954, 15.00000000000002842 ) ) ;
#3150 = CARTESIAN_POINT ( 'NONE',  ( 1.025207404391860050E-15, 3.458734125000000770, 14.43750000136560452 ) ) ;
#3151 = CARTESIAN_POINT ( 'NONE',  ( -2.828427124746189403, -2.828427124746190735, -2.449999997268812457 ) ) ;
#3152 = CARTESIAN_POINT ( 'NONE',  ( 58.03125000000000711, 11.24264068711929276, 18.00000000000000355 ) ) ;
#3153 = DIRECTION ( 'NONE',  ( -1.000000000000000000, 0.000000000000000000, -0.000000000000000000 ) ) ;
#3154 = CARTESIAN_POINT ( 'NONE',  ( 60.00000000000000711, 12.12132034355963484, 12.87867965644034740 ) ) ;
#3155 = CARTESIAN_POINT ( 'NONE',  ( -1.432654583217641164, -3.458734125000000326, 1.175000001365597013 ) ) ;
#3156 = CARTESIAN_POINT ( 'NONE',  ( -2.441083172237810572, -2.460707566094265442, 2.039999999999996039 ) ) ;
#3157 = DIRECTION ( 'NONE',  ( 0.000000000000000000, -1.000000000000000000, -1.047444401652939849E-14 ) ) ;
#3158 = ORIENTED_EDGE ( 'NONE', *, *, #11859, .T. ) ;
#3159 = CARTESIAN_POINT ( 'NONE',  ( 3.263761790716562139, -8.974600000000002353, 10.00000000000008882 ) ) ;
#3160 = CARTESIAN_POINT ( 'NONE',  ( -1.799999999999996048, 0.000000000000000000, -9.000000000000021316 ) ) ;
#3161 = ORIENTED_EDGE ( 'NONE', *, *, #22071, .T. ) ;
#3162 = CARTESIAN_POINT ( 'NONE',  ( 57.65625000000002132, 7.000000000000003553, 16.24264068711929099 ) ) ;
#3163 = SURFACE_SIDE_STYLE ('',( #8345 ) ) ;
#3164 = CARTESIAN_POINT ( 'NONE',  ( -4.000000000000000888, 1.656854249492380804, -1.637499997268811569 ) ) ;
#3165 = DIRECTION ( 'NONE',  ( -1.000000000000000000, 0.000000000000000000, 0.000000000000000000 ) ) ;
#3166 = EDGE_LOOP ( 'NONE', ( #1522, #12488, #16609, #3193 ) ) ;
#3167 = EDGE_LOOP ( 'NONE', ( #14963, #4236, #3384, #15830 ) ) ;
#3168 =( BOUNDED_CURVE ( )  B_SPLINE_CURVE ( 2, ( #7000, #18016, #1470, #23150, #17669, #5313, #3037, #14319, #19915 ),
 .UNSPECIFIED., .F., .F. ) 
 B_SPLINE_CURVE_WITH_KNOTS ( ( 3, 2, 2, 2, 3 ),
 ( 0.8124999999999993339, 0.8281249999999992228, 0.8437499999999991118, 0.8593749999999991118, 0.8749999999999990008 ),
 .UNSPECIFIED. ) 
 CURVE ( )  GEOMETRIC_REPRESENTATION_ITEM ( )  RATIONAL_B_SPLINE_CURVE ( ( 1.000000000000003331, 0.9238795325112835188, 1.000000000000000000, 0.9238795325112867385, 1.000000000000000000, 0.9238795325112867385, 1.000000000000000000, 0.9238795325112916235, 0.9999999999999951150 ) ) 
 REPRESENTATION_ITEM ( '' )  );
#3169 = EDGE_CURVE ( 'NONE', #3905, #11172, #20295, .T. ) ;
#3170 = CARTESIAN_POINT ( 'NONE',  ( -6.989194030332740226, -11.25000000000000355, 5.000000000000079936 ) ) ;
#3171 = LINE ( 'NONE', #12076, #22088 ) ;
#3172 = VERTEX_POINT ( 'NONE', #14715 ) ;
#3173 = CARTESIAN_POINT ( 'NONE',  ( 0.5449313310647804220, 4.304185902836899835, -3.316620875263383894 ) ) ;
#3174 = LINE ( 'NONE', #19020, #6016 ) ;
#3175 = ORIENTED_EDGE ( 'NONE', *, *, #16288, .F. ) ;
#3176 = EDGE_CURVE ( 'NONE', #9843, #3750, #11234, .T. ) ;
#3177 = DIRECTION ( 'NONE',  ( 0.000000000000000000, 0.000000000000000000, -1.000000000000000000 ) ) ;
#3178 = CIRCLE ( 'NONE', #12771, 4.000000000000000000 ) ;
#3179 = CARTESIAN_POINT ( 'NONE',  ( 71.64999999999997726, 11.03553390593273598, 17.50000000000000355 ) ) ;
#3180 = CIRCLE ( 'NONE', #7789, 4.000000000000001776 ) ;
#3181 = CARTESIAN_POINT ( 'NONE',  ( 44.09522139676619901, -9.000000000000003553, 10.00454388062671640 ) ) ;
#3182 = CARTESIAN_POINT ( 'NONE',  ( 69.40000000218495302, 9.999999999999998224, 17.49999999999999645 ) ) ;
#3183 = CARTESIAN_POINT ( 'NONE',  ( 56.84606816583843880, 8.411196891453267099, 19.02818770551464667 ) ) ;
#3184 = CARTESIAN_POINT ( 'NONE',  ( -1.432654583217640942, -3.458734124999999882, 3.925000001365594127 ) ) ;
#3185 = CARTESIAN_POINT ( 'NONE',  ( 2.445694354108821411, 2.445694354108820523, 14.06250000136560452 ) ) ;
#3186 = CARTESIAN_POINT ( 'NONE',  ( 27.56832511966726784, -11.25000000000000355, 10.00000000000008882 ) ) ;
#3187 = VECTOR ( 'NONE', #12322, 1000.000000000000114 ) ;
#3188 = CARTESIAN_POINT ( 'NONE',  ( 54.99999999999996447, 15.00000000000000000, 5.000000000000003553 ) ) ;
#3189 = ORIENTED_EDGE ( 'NONE', *, *, #20301, .T. ) ;
#3190 = CARTESIAN_POINT ( 'NONE',  ( -1.237965327229626045, 3.704993550908596056, 2.039999999999998703 ) ) ;
#3191 = CARTESIAN_POINT ( 'NONE',  ( 68.39999999999999147, 11.76776695296636888, 16.76776695296636532 ) ) ;
#3192 = FACE_BOUND ( 'NONE', #1637, .T. ) ;
#3193 = ORIENTED_EDGE ( 'NONE', *, *, #20000, .T. ) ;
#3194 = EDGE_CURVE ( 'NONE', #19779, #6822, #9209, .T. ) ;
#3195 = CARTESIAN_POINT ( 'NONE',  ( 0.000000000000000000, 9.314797388894893615, 1.239665997526919083 ) ) ;
#3196 = CARTESIAN_POINT ( 'NONE',  ( -67.59999999999999432, 11.76776695296636888, 16.76776695296636532 ) ) ;
#3197 = ADVANCED_FACE ( 'NONE', ( #14600 ), #5467, .T. ) ;
#3198 = CARTESIAN_POINT ( 'NONE',  ( 59.53125000000000711, 11.65685424949239923, 18.99999999999998934 ) ) ;
#3199 = ORIENTED_EDGE ( 'NONE', *, *, #13220, .T. ) ;
#3200 = CARTESIAN_POINT ( 'NONE',  ( -69.64999999999997726, 8.964466094067285340, 12.49999999999996980 ) ) ;
#3201 = ORIENTED_EDGE ( 'NONE', *, *, #6885, .F. ) ;
#3202 = CARTESIAN_POINT ( 'NONE',  ( 55.40625000000000000, 13.99999999999999289, 13.34314575050759544 ) ) ;
#3203 = EDGE_CURVE ( 'NONE', #13418, #17227, #7176, .T. ) ;
#3204 = CARTESIAN_POINT ( 'NONE',  ( 66.45000000218495018, 7.499999999999995559, 13.96446609406725692 ) ) ;
#3205 = EDGE_CURVE ( 'NONE', #1359, #20184, #3438, .T. ) ;
#3206 = CIRCLE ( 'NONE', #20788, 10.00000000000000178 ) ;
#3207 = FACE_OUTER_BOUND ( 'NONE', #3469, .T. ) ;
#3208 = CARTESIAN_POINT ( 'NONE',  ( 72.50000000000000000, 9.999999999999998224, 12.49999999999999289 ) ) ;
#3209 = PLANE ( 'NONE',  #14907 ) ;
#3210 = VERTEX_POINT ( 'NONE', #20057 ) ;
#3211 = CARTESIAN_POINT ( 'NONE',  ( 2.500000000000000000, 2.357898499370431722, -2.818925648462311528E-15 ) ) ;
#3212 = LINE ( 'NONE', #3333, #21746 ) ;
#3213 = CARTESIAN_POINT ( 'NONE',  ( 66.25000000109245946, 9.999999999999998224, 12.93301269999999192 ) ) ;
#3214 = CARTESIAN_POINT ( 'NONE',  ( 3.458734125000002546, -1.432654583217639610, 18.12500000136560274 ) ) ;
#3215 = CYLINDRICAL_SURFACE ( 'NONE', #16254, 2.500000000000002220 ) ;
#3216 = CYLINDRICAL_SURFACE ( 'NONE', #17277, 8.749000000000002331 ) ;
#3217 = ORIENTED_EDGE ( 'NONE', *, *, #3968, .F. ) ;
#3218 = CARTESIAN_POINT ( 'NONE',  ( 2.828427124746190735, -2.828427124746189847, -2.324999999999998845 ) ) ;
#3219 = CARTESIAN_POINT ( 'NONE',  ( 56.06250000000000000, 6.999999999999997335, 15.00000000000000533 ) ) ;
#3220 = EDGE_CURVE ( 'NONE', #3825, #18250, #1977, .T. ) ;
#3221 = CARTESIAN_POINT ( 'NONE',  ( -15.58579410928343911, -8.974600000000002353, 5.000000000000079936 ) ) ;
#3222 = DIRECTION ( 'NONE',  ( 0.000000000000000000, 0.000000000000000000, 1.000000000000000000 ) ) ;
#3223 = VERTEX_POINT ( 'NONE', #12697 ) ;
#3224 = CARTESIAN_POINT ( 'NONE',  ( 0.000000000000000000, 0.000000000000000000, 0.000000000000000000 ) ) ;
#3225 = CARTESIAN_POINT ( 'NONE',  ( 6.353591512924457348E-16, -3.458734125000000326, -3.012499998634404541 ) ) ;
#3226 = CARTESIAN_POINT ( 'NONE',  ( -90.00000000000000000, 0.000000000000000000, 0.000000000000000000 ) ) ;
#3227 = AXIS2_PLACEMENT_3D ( 'NONE', #9882, #22550, #13480 ) ;
#3228 = EDGE_CURVE ( 'NONE', #7815, #1384, #5586, .T. ) ;
#3229 = ORIENTED_EDGE ( 'NONE', *, *, #13078, .T. ) ;
#3230 = CARTESIAN_POINT ( 'NONE',  ( -4.211140560182196957, 2.431303136016537803, -3.745885042887433514 ) ) ;
#3231 = ORIENTED_EDGE ( 'NONE', *, *, #2088, .F. ) ;
#3232 = DIRECTION ( 'NONE',  ( 1.000000000000000000, 0.000000000000000000, 0.000000000000000000 ) ) ;
#3233 = ORIENTED_EDGE ( 'NONE', *, *, #18520, .T. ) ;
#3234 = CARTESIAN_POINT ( 'NONE',  ( -1.432654583217639832, -3.458734125000000326, 10.87500000136560452 ) ) ;
#3235 = ADVANCED_FACE ( 'NONE', ( #20175 ), #19951, .F. ) ;
#3236 = CYLINDRICAL_SURFACE ( 'NONE', #16864, 8.749000000000002331 ) ;
#3237 = ADVANCED_FACE ( 'NONE', ( #16376 ), #7404, .T. ) ;
#3238 = CARTESIAN_POINT ( 'NONE',  ( -68.15000000218495302, 8.964466094067214286, 12.50000000000004086 ) ) ;
#3239 = CARTESIAN_POINT ( 'NONE',  ( 67.15000000109247935, 11.46158073645647235, 16.46158073645647235 ) ) ;
#3240 = LINE ( 'NONE', #5156, #6403 ) ;
#3241 = AXIS2_PLACEMENT_3D ( 'NONE', #14155, #12486, #5035 ) ;
#3242 = VECTOR ( 'NONE', #12419, 1000.000000000000000 ) ;
#3243 = CARTESIAN_POINT ( 'NONE',  ( -70.64999999999999147, 12.50000000000000000, 13.96446609406725869 ) ) ;
#3244 = AXIS2_PLACEMENT_3D ( 'NONE', #7778, #9452, #13415 ) ;
#3245 = DIRECTION ( 'NONE',  ( 1.000000000000000000, -0.000000000000000000, -0.000000000000000000 ) ) ;
#3246 = CARTESIAN_POINT ( 'NONE',  ( 59.99999999999182165, 10.93426768979392349, 18.41713329524482390 ) ) ;
#3247 = CARTESIAN_POINT ( 'NONE',  ( 3.458734125000001214, -1.432654583217639610, 1.425000001365596791 ) ) ;
#3248 = CARTESIAN_POINT ( 'NONE',  ( -17.30284271966725029, -11.25000000000000355, 5.000000000000079936 ) ) ;
#3249 = CARTESIAN_POINT ( 'NONE',  ( 67.99999999999998579, 8.232233047033629347, 13.23223304703362402 ) ) ;
#3250 = CARTESIAN_POINT ( 'NONE',  ( 1.432654583217643163, -3.458734124999999437, 18.75000000136560274 ) ) ;
#3251 = LINE ( 'NONE', #16201, #11133 ) ;
#3252 = EDGE_LOOP ( 'NONE', ( #9859, #14478 ) ) ;
#3253 = DIRECTION ( 'NONE',  ( 0.000000000000000000, 1.000000000000000000, 0.000000000000000000 ) ) ;
#3254 = ORIENTED_EDGE ( 'NONE', *, *, #9004, .F. ) ;
#3255 = CARTESIAN_POINT ( 'NONE',  ( 59.59143183416158962, 11.72490539043799984, 11.02818770551463246 ) ) ;
#3256 = CARTESIAN_POINT ( 'NONE',  ( -66.10000000109248219, 10.85617417291294551, 12.93301269999999370 ) ) ;
#3257 = CARTESIAN_POINT ( 'NONE',  ( 70.00000000000000000, -10.00000000000000000, 14.99999999999999645 ) ) ;
#3258 = CARTESIAN_POINT ( 'NONE',  ( -1.432654583217640276, 3.458734125000000326, -2.449999998634404541 ) ) ;
#3259 = ORIENTED_EDGE ( 'NONE', *, *, #19086, .T. ) ;
#3260 = DIRECTION ( 'NONE',  ( 4.625929269271486900E-16, -1.000000000000000000, -5.665129472695380173E-32 ) ) ;
#3261 = VECTOR ( 'NONE', #12153, 1000.000000000000000 ) ;
#3262 = ORIENTED_EDGE ( 'NONE', *, *, #1139, .F. ) ;
#3263 = AXIS2_PLACEMENT_3D ( 'NONE', #15448, #22715, #20682 ) ;
#3264 = DIRECTION ( 'NONE',  ( 0.000000000000000000, 0.000000000000000000, -1.000000000000000000 ) ) ;
#3265 = ORIENTED_EDGE ( 'NONE', *, *, #4531, .T. ) ;
#3266 = ADVANCED_FACE ( 'NONE', ( #3900 ), #18164, .T. ) ;
#3267 = CARTESIAN_POINT ( 'NONE',  ( 53.37731816583844591, 7.830560233210212218, 12.92679907967049679 ) ) ;
#3268 = ADVANCED_FACE ( 'NONE', ( #18398 ), #13037, .F. ) ;
#3269 = CARTESIAN_POINT ( 'NONE',  ( -66.95000000218496439, 11.03553390593273598, 17.50000000000000355 ) ) ;
#3270 = CARTESIAN_POINT ( 'NONE',  ( 36.99310306966726358, -11.25000000000000355, 5.000000000000079936 ) ) ;
#3271 = AXIS2_PLACEMENT_3D ( 'NONE', #809, #13421, #2722 ) ;
#3272 = DIRECTION ( 'NONE',  ( 0.000000000000000000, 0.000000000000000000, 1.000000000000000000 ) ) ;
#3273 =( BOUNDED_SURFACE ( )  B_SPLINE_SURFACE ( 1, 2, ( 
 ( #1934, #23624, #5653, #7236, #139, #5421, #9276, #16561, #7468, #14788, #22036, #12987, #11308, #13222, #7713, #11433, #11670, #20726, #20608, #15141, #614, #9860, #18939, #8069, #22163, #17158, #5780, #15028, #15260, #2524, #18705, #6014, #20364, #7940, #4330, #19057, #13341, #18584, #11784, #251, #4449, #13571, #20840, #3974, #22282, #2410, #736, #15384, #2165, #22406, #9743, #6252, #7823, #22528, #22647, #4217, #5898, #9386, #16680, #14905, #6140, #11556, #7587, #13108, #18825, #13465, #17037, #9503, #16800, #381, #20490, #4091, #9633, #2296, #16923, #500, #19177, #2648, #20952, #5041, #17280, #2993, #23228, #12372, #14162, #4573, #8535, #2760, #6838, #6375, #2873, #19284, #23006, #4684, #848, #8421, #10221, #9989, #11907, #1197, #6495, #15945, #21425, #10461, #961, #12017, #8179, #21182, #22763, #13928, #15841, #10103, #13817, #8294, #17511, #4920, #14035, #4799, #15734, #15614, #15493, #12255, #21297, #13690, #1309, #17392, #22884, #21076, #19523, #1080, #6612, #12132, #17743, #19398, #10346, #17635, #23111, #6723, #3121, #8645, #10926, #3234, #19985, #14755, #5394, #14524, #3699, #9129, #16419 ),
 ( #21543, #5626, #7441, #14282, #5152, #16185, #10695, #19875, #16308, #12494, #1906, #19755, #1671, #20099, #1423, #11039, #5273, #7083, #12734, #14400, #1552, #18207, #18324, #18088, #108, #22011, #17974, #3588, #6965, #21787, #1785, #8766, #17854, #1, #19636, #3355, #10583, #9249, #16533, #16070, #12615, #7332, #21663, #14638, #23360, #8891, #23474, #3479, #10816, #23595, #21898, #9012, #7208, #5507, #12840, #698, #11164, #11275, #16647, #18438, #3828, #20576, #14875, #9604, #11528, #13192, #2136, #9712, #18549, #9356, #18674, #4062, #225, #7796, #22619, #22490, #5750, #15002, #18907, #8033, #9829, #7554, #11640, #2263, #16896, #7684, #13435, #22253, #2015, #3941, #12957, #5864, #22133, #16768, #15111, #18799, #13079, #20219, #471, #20456, #20335, #22371, #20697, #6103, #582, #4304, #17123, #15352, #11396, #5982, #9471, #13306, #4184, #2382, #350, #17008, #7908, #15225, #2493, #821, #16244, #15895, #12315, #11876, #10761, #8837, #17916, #9955, #5213, #18036, #1613, #3063, #16135, #19466, #17249, #17799, #14341, #14101, #16011, #23297, #6224, #8153, #1496, #8955, #21482, #13543, #6907, #20812, #14227 ) ),
 .UNSPECIFIED., .F., .F., .F. ) 
 B_SPLINE_SURFACE_WITH_KNOTS ( ( 2, 2 ),
 ( 3, 2, 2, 2, 2, 2, 2, 2, 2, 2, 2, 2, 2, 2, 2, 2, 2, 2, 2, 2, 2, 2, 2, 2, 2, 2, 2, 2, 2, 2, 2, 2, 2, 2, 2, 2, 2, 2, 2, 2, 2, 2, 2, 2, 2, 2, 2, 2, 2, 2, 2, 2, 2, 2, 2, 2, 2, 2, 2, 2, 2, 2, 2, 2, 2, 2, 2, 2, 2, 2, 2, 2, 2, 2, 3 ),
 ( 0.000000000000000000, 1.000000000000000000 ),
 ( 0.000000000000000000, 0.01250000000000000069, 0.02500000000000000139, 0.03749999999999999861, 0.05000000000000000278, 0.06250000000000000000, 0.07499999999999999722, 0.08749999999999999445, 0.1000000000000000056, 0.1125000000000000028, 0.1250000000000000000, 0.1375000000000000111, 0.1499999999999999944, 0.1625000000000000056, 0.1749999999999999889, 0.1875000000000000000, 0.2000000000000000111, 0.2124999999999999944, 0.2250000000000000056, 0.2374999999999999889, 0.2500000000000000000, 0.2625000000000000111, 0.2750000000000000222, 0.2874999999999999778, 0.2999999999999999889, 0.3125000000000000000, 0.3250000000000000111, 0.3375000000000000222, 0.3499999999999999778, 0.3624999999999999889, 0.3750000000000000000, 0.3875000000000000111, 0.4000000000000000222, 0.4124999999999999778, 0.4249999999999999889, 0.4375000000000000000, 0.4500000000000000111, 0.4625000000000000222, 0.4749999999999999778, 0.4874999999999999889, 0.5000000000000000000, 0.5124999999999999556, 0.5250000000000000222, 0.5374999999999999778, 0.5500000000000000444, 0.5625000000000000000, 0.5749999999999999556, 0.5875000000000000222, 0.5999999999999999778, 0.6125000000000000444, 0.6250000000000000000, 0.6374999999999999556, 0.6500000000000000222, 0.6624999999999999778, 0.6750000000000000444, 0.6875000000000000000, 0.6999999999999999556, 0.7125000000000000222, 0.7249999999999999778, 0.7375000000000000444, 0.7500000000000000000, 0.7624999999999999556, 0.7750000000000000222, 0.7874999999999999778, 0.8000000000000000444, 0.8125000000000000000, 0.8249999999999999556, 0.8375000000000000222, 0.8499999999999999778, 0.8625000000000000444, 0.8750000000000000000, 0.8874999999999999556, 0.9000000000000000222, 0.9124999999999999778, 0.9250000000000000444 ),
 .UNSPECIFIED. ) 
 GEOMETRIC_REPRESENTATION_ITEM ( )  RATIONAL_B_SPLINE_SURFACE ( (
 ( 1.000000000000000000, 0.9238795325112867385, 1.000000000000000000, 0.9238795325112867385, 1.000000000000000000, 0.9238795325112867385, 1.000000000000000000, 0.9238795325112867385, 1.000000000000000000, 0.9238795325112867385, 1.000000000000000000, 0.9238795325112867385, 1.000000000000000000, 0.9238795325112867385, 1.000000000000000000, 0.9238795325112867385, 1.000000000000000000, 0.9238795325112867385, 1.000000000000000000, 0.9238795325112867385, 1.000000000000000000, 0.9238795325112867385, 1.000000000000000000, 0.9238795325112867385, 1.000000000000000000, 0.9238795325112867385, 1.000000000000000000, 0.9238795325112867385, 1.000000000000000000, 0.9238795325112867385, 1.000000000000000000, 0.9238795325112867385, 1.000000000000000000, 0.9238795325112867385, 1.000000000000000000, 0.9238795325112867385, 1.000000000000000000, 0.9238795325112867385, 1.000000000000000000, 0.9238795325112867385, 1.000000000000000000, 0.9238795325112867385, 1.000000000000000000, 0.9238795325112867385, 1.000000000000000000, 0.9238795325112867385, 1.000000000000000000, 0.9238795325112867385, 1.000000000000000000, 0.9238795325112867385, 1.000000000000000000, 0.9238795325112867385, 1.000000000000000000, 0.9238795325112867385, 1.000000000000000000, 0.9238795325112867385, 1.000000000000000000, 0.9238795325112867385, 1.000000000000000000, 0.9238795325112867385, 1.000000000000000000, 0.9238795325112867385, 1.000000000000000000, 0.9238795325112867385, 1.000000000000000000, 0.9238795325112867385, 1.000000000000000000, 0.9238795325112867385, 1.000000000000000000, 0.9238795325112867385, 1.000000000000000000, 0.9238795325112867385, 1.000000000000000000, 0.9238795325112867385, 1.000000000000000000, 0.9238795325112867385, 1.000000000000000000, 0.9238795325112867385, 1.000000000000000000, 0.9238795325112867385, 1.000000000000000000, 0.9238795325112867385, 1.000000000000000000, 0.9238795325112867385, 1.000000000000000000, 0.9238795325112867385, 1.000000000000000000, 0.9238795325112867385, 1.000000000000000000, 0.9238795325112867385, 1.000000000000000000, 0.9238795325112867385, 1.000000000000000000, 0.9238795325112867385, 1.000000000000000000, 0.9238795325112867385, 1.000000000000000000, 0.9238795325112867385, 1.000000000000000000, 0.9238795325112867385, 1.000000000000000000, 0.9238795325112867385, 1.000000000000000000, 0.9238795325112867385, 1.000000000000000000, 0.9238795325112867385, 1.000000000000000000, 0.9238795325112867385, 1.000000000000000000, 0.9238795325112867385, 1.000000000000000000, 0.9238795325112867385, 1.000000000000000000, 0.9238795325112867385, 1.000000000000000000, 0.9238795325112867385, 1.000000000000000000, 0.9238795325112867385, 1.000000000000000000, 0.9238795325112867385, 1.000000000000000000, 0.9238795325112867385, 1.000000000000000000, 0.9238795325112867385, 1.000000000000000000, 0.9238795325112867385, 1.000000000000000000, 0.9238795325112867385, 1.000000000000000000, 0.9238795325112867385, 1.000000000000000000, 0.9238795325112867385, 1.000000000000000000, 0.9238795325112867385, 1.000000000000000000, 0.9238795325112867385, 1.000000000000000000, 0.9238795325112867385, 1.000000000000000000, 0.9238795325112867385, 1.000000000000000000, 0.9238795325112867385, 1.000000000000000000, 0.9238795325112867385, 1.000000000000000000, 0.9238795325112867385, 1.000000000000000000, 0.9238795325112867385, 1.000000000000000000),
 ( 1.000000000000000000, 0.9238795325112867385, 1.000000000000000000, 0.9238795325112867385, 1.000000000000000000, 0.9238795325112867385, 1.000000000000000000, 0.9238795325112867385, 1.000000000000000000, 0.9238795325112867385, 1.000000000000000000, 0.9238795325112867385, 1.000000000000000000, 0.9238795325112867385, 1.000000000000000000, 0.9238795325112867385, 1.000000000000000000, 0.9238795325112867385, 1.000000000000000000, 0.9238795325112867385, 1.000000000000000000, 0.9238795325112867385, 1.000000000000000000, 0.9238795325112867385, 1.000000000000000000, 0.9238795325112867385, 1.000000000000000000, 0.9238795325112867385, 1.000000000000000000, 0.9238795325112867385, 1.000000000000000000, 0.9238795325112867385, 1.000000000000000000, 0.9238795325112867385, 1.000000000000000000, 0.9238795325112867385, 1.000000000000000000, 0.9238795325112867385, 1.000000000000000000, 0.9238795325112867385, 1.000000000000000000, 0.9238795325112867385, 1.000000000000000000, 0.9238795325112867385, 1.000000000000000000, 0.9238795325112867385, 1.000000000000000000, 0.9238795325112867385, 1.000000000000000000, 0.9238795325112867385, 1.000000000000000000, 0.9238795325112867385, 1.000000000000000000, 0.9238795325112867385, 1.000000000000000000, 0.9238795325112867385, 1.000000000000000000, 0.9238795325112867385, 1.000000000000000000, 0.9238795325112867385, 1.000000000000000000, 0.9238795325112867385, 1.000000000000000000, 0.9238795325112867385, 1.000000000000000000, 0.9238795325112867385, 1.000000000000000000, 0.9238795325112867385, 1.000000000000000000, 0.9238795325112867385, 1.000000000000000000, 0.9238795325112867385, 1.000000000000000000, 0.9238795325112867385, 1.000000000000000000, 0.9238795325112867385, 1.000000000000000000, 0.9238795325112867385, 1.000000000000000000, 0.9238795325112867385, 1.000000000000000000, 0.9238795325112867385, 1.000000000000000000, 0.9238795325112867385, 1.000000000000000000, 0.9238795325112867385, 1.000000000000000000, 0.9238795325112867385, 1.000000000000000000, 0.9238795325112867385, 1.000000000000000000, 0.9238795325112867385, 1.000000000000000000, 0.9238795325112867385, 1.000000000000000000, 0.9238795325112867385, 1.000000000000000000, 0.9238795325112867385, 1.000000000000000000, 0.9238795325112867385, 1.000000000000000000, 0.9238795325112867385, 1.000000000000000000, 0.9238795325112867385, 1.000000000000000000, 0.9238795325112867385, 1.000000000000000000, 0.9238795325112867385, 1.000000000000000000, 0.9238795325112867385, 1.000000000000000000, 0.9238795325112867385, 1.000000000000000000, 0.9238795325112867385, 1.000000000000000000, 0.9238795325112867385, 1.000000000000000000, 0.9238795325112867385, 1.000000000000000000, 0.9238795325112867385, 1.000000000000000000, 0.9238795325112867385, 1.000000000000000000, 0.9238795325112867385, 1.000000000000000000, 0.9238795325112867385, 1.000000000000000000, 0.9238795325112867385, 1.000000000000000000, 0.9238795325112867385, 1.000000000000000000, 0.9238795325112867385, 1.000000000000000000, 0.9238795325112867385, 1.000000000000000000, 0.9238795325112867385, 1.000000000000000000, 0.9238795325112867385, 1.000000000000000000, 0.9238795325112867385, 1.000000000000000000, 0.9238795325112867385, 1.000000000000000000, 0.9238795325112867385, 1.000000000000000000, 0.9238795325112867385, 1.000000000000000000, 0.9238795325112867385, 1.000000000000000000) ) ) 
 REPRESENTATION_ITEM ( '' )  SURFACE ( )  );
#3274 = CARTESIAN_POINT ( 'NONE',  ( 1.432654583217643163, -3.458734124999999882, 16.00000000136560629 ) ) ;
#3275 = CARTESIAN_POINT ( 'NONE',  ( 2.828427124746190735, -2.828427124746189847, -2.199999997268812013 ) ) ;
#3276 = CARTESIAN_POINT ( 'NONE',  ( 55.96875000000000000, 6.999999999999992895, 13.75735931288071967 ) ) ;
#3277 = CIRCLE ( 'NONE', #16676, 8.749000000000002331 ) ;
#3278 = CARTESIAN_POINT ( 'NONE',  ( 57.93750000000000000, 10.00000000000000711, 17.99999999999999645 ) ) ;
#3279 = VECTOR ( 'NONE', #16962, 1000.000000000000114 ) ;
#3280 = CARTESIAN_POINT ( 'NONE',  ( -3.458734125000000326, -1.432654583217642497, 0.05000000136559582670 ) ) ;
#3281 = CARTESIAN_POINT ( 'NONE',  ( -3.196266448073070254, -1.341181843264293905, 2.040000000000002256 ) ) ;
#3282 = CARTESIAN_POINT ( 'NONE',  ( -68.34999999999999432, 12.50000000000000000, 16.03553390593273775 ) ) ;
#3283 = ORIENTED_EDGE ( 'NONE', *, *, #20798, .T. ) ;
#3284 = DIRECTION ( 'NONE',  ( 1.000000000000000000, 4.625929269271485914E-16, -1.224646799147353454E-16 ) ) ;
#3285 = DIRECTION ( 'NONE',  ( 1.000000000000000000, 0.000000000000000000, 0.000000000000000000 ) ) ;
#3286 = VERTEX_POINT ( 'NONE', #13150 ) ;
#3287 = CARTESIAN_POINT ( 'NONE',  ( 58.68750000000000000, 9.999999999999989342, 11.99999999999999467 ) ) ;
#3288 = PRESENTATION_STYLE_ASSIGNMENT (( #21473 ) ) ;
#3289 = CARTESIAN_POINT ( 'NONE',  ( -1.656854249492380804, 4.000000000000000000, -1.762499997268811569 ) ) ;
#3290 = FACE_OUTER_BOUND ( 'NONE', #8292, .T. ) ;
#3291 = ORIENTED_EDGE ( 'NONE', *, *, #9103, .T. ) ;
#3292 = ORIENTED_EDGE ( 'NONE', *, *, #1910, .F. ) ;
#3293 = DIRECTION ( 'NONE',  ( -1.224646799147353207E-16, 0.000000000000000000, -1.000000000000000000 ) ) ;
#3294 = FACE_OUTER_BOUND ( 'NONE', #10599, .T. ) ;
#3295 = ORIENTED_EDGE ( 'NONE', *, *, #17438, .F. ) ;
#3296 = FACE_OUTER_BOUND ( 'NONE', #11836, .T. ) ;
#3297 = CARTESIAN_POINT ( 'NONE',  ( 72.50000000000000000, 9.999999999999998224, 14.99999999999999645 ) ) ;
#3298 = ORIENTED_EDGE ( 'NONE', *, *, #23598, .T. ) ;
#3299 = CARTESIAN_POINT ( 'NONE',  ( 66.55000000109247082, 8.538419263543522320, 16.46158073645647235 ) ) ;
#3300 = CARTESIAN_POINT ( 'NONE',  ( 71.09999999999999432, 7.499999999999996447, 14.99999999999999645 ) ) ;
#3301 = ORIENTED_EDGE ( 'NONE', *, *, #15537, .T. ) ;
#3302 = EDGE_CURVE ( 'NONE', #17674, #15665, #21861, .T. ) ;
#3303 = CARTESIAN_POINT ( 'NONE',  ( 19.99999999999998934, 9.999999999999964473, -50.00000000000000000 ) ) ;
#3304 = CARTESIAN_POINT ( 'NONE',  ( 51.37500000000000711, 7.171572875253794166, 12.17157287525381726 ) ) ;
#3305 = CARTESIAN_POINT ( 'NONE',  ( -2.117863837641485618E-16, 3.458734125000000326, 4.487500001365595459 ) ) ;
#3306 = SURFACE_STYLE_FILL_AREA ( #19702 ) ;
#3307 = CARTESIAN_POINT ( 'NONE',  ( -3.458734124999998993, 0.000000000000000000, 15.43750000136560452 ) ) ;
#3308 = CARTESIAN_POINT ( 'NONE',  ( -18.73663160323380339, -9.000000000000003553, 10.00000000000008882 ) ) ;
#3309 = DIRECTION ( 'NONE',  ( -1.000000000000000000, -0.000000000000000000, -0.000000000000000000 ) ) ;
#3310 = EDGE_LOOP ( 'NONE', ( #4795, #8287, #22660, #12729, #7641 ) ) ;
#3311 = CARTESIAN_POINT ( 'NONE',  ( -3.429173157536499428, 1.281533049792265677, 2.039999999999997371 ) ) ;
#3312 = CARTESIAN_POINT ( 'NONE',  ( -6.499999999999999112, 3.145973671264225668, -3.294612376748628613 ) ) ;
#3313 = CARTESIAN_POINT ( 'NONE',  ( 4.000000000000000888, 4.898587196589412829E-16, 20.00000000000001066 ) ) ;
#3314 = VERTEX_POINT ( 'NONE', #18508 ) ;
#3315 = CARTESIAN_POINT ( 'NONE',  ( -90.00000000000000000, 1.102182119232620672E-15, 9.000000000000021316 ) ) ;
#3316 = CARTESIAN_POINT ( 'NONE',  ( 71.30000000109248504, 9.143825827087049163, 17.06698729999999742 ) ) ;
#3317 = ORIENTED_EDGE ( 'NONE', *, *, #14577, .F. ) ;
#3318 = ORIENTED_EDGE ( 'NONE', *, *, #5565, .T. ) ;
#3319 = LINE ( 'NONE', #15809, #2239 ) ;
#3320 = ORIENTED_EDGE ( 'NONE', *, *, #9461, .F. ) ;
#3321 = CARTESIAN_POINT ( 'NONE',  ( 51.93750000000000711, 10.00000000000001776, 18.99999999999999645 ) ) ;
#3322 = CARTESIAN_POINT ( 'NONE',  ( 68.15000000218495302, 8.964466094067258695, 12.49999999999999289 ) ) ;
#3323 = VECTOR ( 'NONE', #3284, 1000.000000000000000 ) ;
#3324 = DIRECTION ( 'NONE',  ( -1.000000000000000000, 0.000000000000000000, 0.000000000000000000 ) ) ;
#3325 = LINE ( 'NONE', #3208, #17521 ) ;
#3326 = DIRECTION ( 'NONE',  ( -0.000000000000000000, -0.000000000000000000, -1.000000000000000000 ) ) ;
#3327 = EDGE_LOOP ( 'NONE', ( #7869, #12393, #2219, #4023 ) ) ;
#3328 = VECTOR ( 'NONE', #8213, 1000.000000000000000 ) ;
#3329 = EDGE_CURVE ( 'NONE', #9434, #23001, #16265, .T. ) ;
#3330 = CARTESIAN_POINT ( 'NONE',  ( -4.211140560182196957, 2.431303136016537803, -3.745885042887433514 ) ) ;
#3331 = EDGE_CURVE ( 'NONE', #2257, #7929, #16724, .T. ) ;
#3332 = CARTESIAN_POINT ( 'NONE',  ( 60.24768183416157541, 7.123453452023678523, 17.78030770151605822 ) ) ;
#3333 = CARTESIAN_POINT ( 'NONE',  ( 14.99999999999995914, 15.00000000000000000, -20.00000000000000355 ) ) ;
#3334 = CARTESIAN_POINT ( 'NONE',  ( 68.20000000109246230, 10.85617417291294551, 17.06698729999999742 ) ) ;
#3335 = VECTOR ( 'NONE', #2703, 1000.000000000000000 ) ;
#3336 = CARTESIAN_POINT ( 'NONE',  ( -2.445694354108819191, 2.445694354108820523, 17.56250000136560274 ) ) ;
#3337 = LINE ( 'NONE', #5025, #5924 ) ;
#3338 = VECTOR ( 'NONE', #14817, 1000.000000000000000 ) ;
#3339 = LINE ( 'NONE', #21528, #20284 ) ;
#3340 = EDGE_LOOP ( 'NONE', ( #4442, #9333, #23525, #23681 ) ) ;
#3341 = CARTESIAN_POINT ( 'NONE',  ( 1.520000000000000462, 0.000000000000000000, 0.000000000000000000 ) ) ;
#3342 = CARTESIAN_POINT ( 'NONE',  ( 57.00000000000000000, 12.12132034355963484, 12.87867965644034740 ) ) ;
#3343 = CARTESIAN_POINT ( 'NONE',  ( 9.920644283265380691E-16, 4.000000000000000000, 10.87500000273119660 ) ) ;
#3344 = DIRECTION ( 'NONE',  ( 1.000000000000000000, 0.000000000000000000, 0.000000000000000000 ) ) ;
#3345 = EDGE_CURVE ( 'NONE', #15758, #16269, #14961, .T. ) ;
#3346 = VERTEX_POINT ( 'NONE', #13270 ) ;
#3347 = PLANE ( 'NONE',  #14370 ) ;
#3348 = CARTESIAN_POINT ( 'NONE',  ( -1.432654583217640942, -3.458734124999999882, -3.074999998634404541 ) ) ;
#3349 = DIRECTION ( 'NONE',  ( 0.3420201433256622181, 0.9396926207859107594, -6.162975822039141593E-32 ) ) ;
#3350 = ORIENTED_EDGE ( 'NONE', *, *, #4830, .T. ) ;
#3351 = DIRECTION ( 'NONE',  ( 0.000000000000000000, 0.000000000000000000, -1.000000000000000000 ) ) ;
#3352 = ORIENTED_EDGE ( 'NONE', *, *, #21094, .T. ) ;
#3353 = CARTESIAN_POINT ( 'NONE',  ( 0.000000000000000000, 0.000000000000000000, 1.734723475976807094E-15 ) ) ;
#3354 = ORIENTED_EDGE ( 'NONE', *, *, #3511, .T. ) ;
#3355 = CARTESIAN_POINT ( 'NONE',  ( -1.656854249492379250, 4.000000000000000000, 17.81250000000001421 ) ) ;
#3356 = CARTESIAN_POINT ( 'NONE',  ( -4.000000000000000000, 2.309401076758498483, -0.4999999999999927280 ) ) ;
#3357 = AXIS2_PLACEMENT_3D ( 'NONE', #6341, #15581, #17478 ) ;
#3358 = DIRECTION ( 'NONE',  ( 1.000000000000000000, -0.000000000000000000, -0.000000000000000000 ) ) ;
#3359 = ADVANCED_FACE ( 'NONE', ( #2568 ), #5479, .F. ) ;
#3360 = DIRECTION ( 'NONE',  ( -1.000000000000000000, 0.000000000000000000, 0.000000000000000000 ) ) ;
#3361 = LINE ( 'NONE', #8653, #12140 ) ;
#3362 = CARTESIAN_POINT ( 'NONE',  ( -68.29999999999999716, 12.50000000000000000, 14.99999999999999645 ) ) ;
#3363 = EDGE_CURVE ( 'NONE', #9768, #2705, #4914, .T. ) ;
#3364 = CARTESIAN_POINT ( 'NONE',  ( 60.00000000000000711, 12.67839003132778686, 16.61512380723988258 ) ) ;
#3365 = AXIS2_PLACEMENT_3D ( 'NONE', #16417, #23697, #11527 ) ;
#3366 = CARTESIAN_POINT ( 'NONE',  ( 3.458734125000001214, -1.432654583217639610, 0.4250000013655961251 ) ) ;
#3367 = LINE ( 'NONE', #23016, #2262 ) ;
#3368 = FACE_OUTER_BOUND ( 'NONE', #10344, .T. ) ;
#3369 = CARTESIAN_POINT ( 'NONE',  ( -2.445694354108819191, 2.445694354108820523, 19.31250000136560629 ) ) ;
#3370 = DIRECTION ( 'NONE',  ( 0.000000000000000000, 0.000000000000000000, 1.000000000000000000 ) ) ;
#3371 = ADVANCED_FACE ( 'NONE', ( #18083 ), #7201, .T. ) ;
#3372 = AXIS2_PLACEMENT_3D ( 'NONE', #1020, #8703, #17684 ) ;
#3373 = EDGE_CURVE ( 'NONE', #13272, #19009, #23353, .T. ) ;
#3374 = ORIENTED_EDGE ( 'NONE', *, *, #15548, .T. ) ;
#3375 = TOROIDAL_SURFACE ( 'NONE', #3739, 4.000000000000000000, 0.2500000000000000000 ) ;
#3376 = CARTESIAN_POINT ( 'NONE',  ( 2.828427124746192067, -2.828427124746189847, 14.50000000273119660 ) ) ;
#3377 = ORIENTED_EDGE ( 'NONE', *, *, #3793, .T. ) ;
#3378 = CARTESIAN_POINT ( 'NONE',  ( 56.96643183416158251, 6.028187705514633343, 13.27509460956200016 ) ) ;
#3379 = CARTESIAN_POINT ( 'NONE',  ( -67.45000000109246230, 7.933012699999995476, 14.99999999999999645 ) ) ;
#3380 = AXIS2_PLACEMENT_3D ( 'NONE', #19419, #11928, #2669 ) ;
#3381 = CARTESIAN_POINT ( 'NONE',  ( 19.99999999999999645, 4.500000000000003553, -50.00000000000000000 ) ) ;
#3382 = ORIENTED_EDGE ( 'NONE', *, *, #11929, .T. ) ;
#3383 = CARTESIAN_POINT ( 'NONE',  ( -65.00000000000000000, 9.999999999999998224, 12.49999999999999289 ) ) ;
#3384 = ORIENTED_EDGE ( 'NONE', *, *, #20801, .F. ) ;
#3385 = ORIENTED_EDGE ( 'NONE', *, *, #4860, .F. ) ;
#3386 = CARTESIAN_POINT ( 'NONE',  ( 59.90625000000000711, 12.99999999999999645, 13.75735931288070191 ) ) ;
#3387 = VECTOR ( 'NONE', #10932, 1000.000000000000000 ) ;
#3388 = CARTESIAN_POINT ( 'NONE',  ( -65.40000000218495302, 9.999999999999998224, 17.49999999999999645 ) ) ;
#3389 = CARTESIAN_POINT ( 'NONE',  ( -11.01965741966725076, -11.25000000000000355, 10.00000000000008882 ) ) ;
#3390 = LINE ( 'NONE', #21457, #12606 ) ;
#3391 = CARTESIAN_POINT ( 'NONE',  ( -2.445694354108819191, 2.445694354108820523, 15.56250000136560629 ) ) ;
#3392 = CARTESIAN_POINT ( 'NONE',  ( 7.347880794884118750E-16, -4.000000000000000000, -2.324999997268812013 ) ) ;
#3393 = CARTESIAN_POINT ( 'NONE',  ( 55.78125000000000000, 8.757359312880703683, 11.99999999999999822 ) ) ;
#3394 = FACE_OUTER_BOUND ( 'NONE', #5114, .T. ) ;
#3395 = CARTESIAN_POINT ( 'NONE',  ( 50.37731816583844591, 7.830560233210212218, 12.92679907967049679 ) ) ;
#3396 = CARTESIAN_POINT ( 'NONE',  ( 2.445694354108820967, -2.445694354108820079, -2.637499998634404097 ) ) ;
#3397 = CARTESIAN_POINT ( 'NONE',  ( -2.828427124746188515, -2.828427124746190735, 18.25000000273119483 ) ) ;
#3399 = EDGE_CURVE ( 'NONE', #17589, #22866, #10576, .T. ) ;
#3398 = VECTOR ( 'NONE', #13906, 1000.000000000000000 ) ;
#3400 = DIRECTION ( 'NONE',  ( 0.000000000000000000, 0.000000000000000000, 1.000000000000000000 ) ) ;
#3401 = EDGE_CURVE ( 'NONE', #10887, #19450, #14393, .T. ) ;
#3402 = AXIS2_PLACEMENT_3D ( 'NONE', #3211, #17832, #15591 ) ;
#3403 = VERTEX_POINT ( 'NONE', #16063 ) ;
#3404 = CARTESIAN_POINT ( 'NONE',  ( 70.50000000000000000, 9.999999999999998224, 12.49999999999999289 ) ) ;
#3405 = FACE_BOUND ( 'NONE', #3874, .T. ) ;
#3406 = ORIENTED_EDGE ( 'NONE', *, *, #1894, .T. ) ;
#3407 = FACE_OUTER_BOUND ( 'NONE', #14859, .T. ) ;
#3408 = CARTESIAN_POINT ( 'NONE',  ( 7.347880794884118750E-16, -4.000000000000000000, 1.675000002731187987 ) ) ;
#3409 = DIRECTION ( 'NONE',  ( -0.5000000000000006661, 0.8660254037844383745, 0.000000000000000000 ) ) ;
#3410 = EDGE_LOOP ( 'NONE', ( #6581, #15026, #15750, #833, #17567, #4157, #18580, #9790, #6032, #3054, #8869, #4896 ) ) ;
#3411 = AXIS2_PLACEMENT_3D ( 'NONE', #12753, #21445, #7356 ) ;
#3412 = CARTESIAN_POINT ( 'NONE',  ( 9.920644283265380691E-16, 4.000000000000000000, 17.75000000000000711 ) ) ;
#3413 = ORIENTED_EDGE ( 'NONE', *, *, #23257, .T. ) ;
#3414 = DIRECTION ( 'NONE',  ( 0.000000000000000000, 0.000000000000000000, -1.000000000000000000 ) ) ;
#3415 = VECTOR ( 'NONE', #12382, 1000.000000000000000 ) ;
#3416 = CARTESIAN_POINT ( 'NONE',  ( 2.828427124746189847, 2.828427124746190291, -2.949999997268812901 ) ) ;
#3417 = ORIENTED_EDGE ( 'NONE', *, *, #15818, .T. ) ;
#3418 = FACE_OUTER_BOUND ( 'NONE', #19840, .T. ) ;
#3419 = CARTESIAN_POINT ( 'NONE',  ( -35.00000000000000000, 7.500000000000001776, -19.99999999999998934 ) ) ;
#3420 =( BOUNDED_CURVE ( )  B_SPLINE_CURVE ( 2, ( #10724, #20330, #5859, #3822, #9598 ),
 .UNSPECIFIED., .F., .F. ) 
 B_SPLINE_CURVE_WITH_KNOTS ( ( 3, 2, 3 ),
 ( 0.9000000000000000222, 0.9124999999999999778, 0.9250000000000000444 ),
 .UNSPECIFIED. ) 
 CURVE ( )  GEOMETRIC_REPRESENTATION_ITEM ( )  RATIONAL_B_SPLINE_CURVE ( ( 1.000000000000000000, 0.9238795325112867385, 1.000000000000000000, 0.9238795325112867385, 1.000000000000000000 ) ) 
 REPRESENTATION_ITEM ( '' )  );
#3421 = ORIENTED_EDGE ( 'NONE', *, *, #7065, .F. ) ;
#3422 = CONICAL_SURFACE ( 'NONE', #17195, 6.500000000000000888, 1.047197551196596521 ) ;
#3423 = CARTESIAN_POINT ( 'NONE',  ( 3.999999999999999112, 1.941961291383486277, -0.3515519931180248192 ) ) ;
#3424 = VECTOR ( 'NONE', #18387, 1000.000000000000000 ) ;
#3425 = CARTESIAN_POINT ( 'NONE',  ( 71.95000000000001705, 7.499999999999995559, 13.96446609406725692 ) ) ;
#3426 = CARTESIAN_POINT ( 'NONE',  ( -3.999999999999999112, 0.000000000000000000, 17.12500000273119838 ) ) ;
#3427 = CARTESIAN_POINT ( 'NONE',  ( 4.999999999999999112, 10.90201369670498721, -1.464956435139581403 ) ) ;
#3428 = VECTOR ( 'NONE', #2448, 1000.000000000000114 ) ;
#3429 = CARTESIAN_POINT ( 'NONE',  ( 59.00231816583843170, 12.78030770151603868, 12.12345345202365188 ) ) ;
#3430 = CARTESIAN_POINT ( 'NONE',  ( 6.353591512924457348E-16, -3.458734125000000326, -0.01249999863440348635 ) ) ;
#3431 = PLANE ( 'NONE',  #7637 ) ;
#3432 = CARTESIAN_POINT ( 'NONE',  ( -1.432654583217638944, 3.458734125000000326, 16.25000000136560629 ) ) ;
#3433 = LINE ( 'NONE', #3774, #20450 ) ;
#3434 = DIRECTION ( 'NONE',  ( 1.000000000000000000, 0.000000000000000000, -1.224646799147353207E-16 ) ) ;
#3435 = ORIENTED_EDGE ( 'NONE', *, *, #23408, .F. ) ;
#3436 = CARTESIAN_POINT ( 'NONE',  ( -3.478414791966562891, -0.5482830432473079219, 2.039999999999999591 ) ) ;
#3437 = DIRECTION ( 'NONE',  ( -1.000000000000000000, -0.000000000000000000, -0.000000000000000000 ) ) ;
#3438 = LINE ( 'NONE', #22211, #23514 ) ;
#3439 = ORIENTED_EDGE ( 'NONE', *, *, #11322, .T. ) ;
#3440 = ORIENTED_EDGE ( 'NONE', *, *, #16382, .F. ) ;
#3441 = AXIS2_PLACEMENT_3D ( 'NONE', #8363, #15681, #22826 ) ;
#3442 = DIRECTION ( 'NONE',  ( 0.000000000000000000, 0.3090169943749412895, 0.9510565162951555296 ) ) ;
#3443 = DIRECTION ( 'NONE',  ( 0.000000000000000000, 1.000000000000000000, -1.224646799147353207E-16 ) ) ;
#3444 = EDGE_LOOP ( 'NONE', ( #13156, #7205, #11208, #12331 ) ) ;
#3445 = CARTESIAN_POINT ( 'NONE',  ( -6.499999999999999112, -0.6341575537611441327, 4.540096597283048831E-16 ) ) ;
#3446 = EDGE_LOOP ( 'NONE', ( #18459, #7578, #16120, #14007 ) ) ;
#3447 = AXIS2_PLACEMENT_3D ( 'NONE', #8852, #1628, #8972 ) ;
#3448 = EDGE_CURVE ( 'NONE', #10320, #23289, #12456, .T. ) ;
#3449 = CARTESIAN_POINT ( 'NONE',  ( 53.53125000000000000, 11.65685424949239923, 18.99999999999998934 ) ) ;
#3450 = VECTOR ( 'NONE', #12747, 1000.000000000000000 ) ;
#3451 = CARTESIAN_POINT ( 'NONE',  ( 68.60000000218495586, 9.999999999999998224, 17.49999999999999645 ) ) ;
#3452 = CARTESIAN_POINT ( 'NONE',  ( 65.00000000000000000, 9.999999999999998224, 14.99999999999999645 ) ) ;
#3453 = FACE_OUTER_BOUND ( 'NONE', #12680, .T. ) ;
#3454 = DIRECTION ( 'NONE',  ( 1.000000000000000000, 0.000000000000000000, 0.000000000000000000 ) ) ;
#3455 = VERTEX_POINT ( 'NONE', #14276 ) ;
#3456 = CARTESIAN_POINT ( 'NONE',  ( -3.999999999999998224, -1.656854249492383246, 16.18750000273119838 ) ) ;
#3457 = CARTESIAN_POINT ( 'NONE',  ( 4.999999999999999112, 9.241976615262133876, 1.699438267350532827 ) ) ;
#3458 = CARTESIAN_POINT ( 'NONE',  ( 57.15393183416157541, 5.971812294485358663, 16.58880310854675599 ) ) ;
#3459 = CARTESIAN_POINT ( 'NONE',  ( -4.000000000000000000, 0.000000000000000000, 0.3000000000000016542 ) ) ;
#3460 = CARTESIAN_POINT ( 'NONE',  ( 19.99999999999998934, 9.999999999999964473, -50.00000000000000000 ) ) ;
#3461 = AXIS2_PLACEMENT_3D ( 'NONE', #21544, #17855, #9250 ) ;
#3462 = LINE ( 'NONE', #10799, #9766 ) ;
#3463 = CARTESIAN_POINT ( 'NONE',  ( 4.999999999999999112, 0.000000000000000000, 0.000000000000000000 ) ) ;
#3464 = ORIENTED_EDGE ( 'NONE', *, *, #6828, .F. ) ;
#3465 = CARTESIAN_POINT ( 'NONE',  ( -1.338706173739542260, 3.195114087442786577, -3.295601554149324652 ) ) ;
#3466 = CARTESIAN_POINT ( 'NONE',  ( 54.65625000000000711, 7.000000000000002665, 16.24264068711929099 ) ) ;
#3467 = CARTESIAN_POINT ( 'NONE',  ( -1.656854249492381248, -3.999999999999999112, 0.6125000027311866546 ) ) ;
#3468 = CARTESIAN_POINT ( 'NONE',  ( -72.29999999999998295, 12.50000000000000000, 14.99999999999999645 ) ) ;
#3469 = EDGE_LOOP ( 'NONE', ( #138, #11067, #4937, #19301 ) ) ;
#3470 = DIRECTION ( 'NONE',  ( 0.000000000000000000, 0.000000000000000000, 1.000000000000000000 ) ) ;
#3471 = CARTESIAN_POINT ( 'NONE',  ( -2.445694354108819635, -2.445694354108820523, -3.137499998634404541 ) ) ;
#3472 = CARTESIAN_POINT ( 'NONE',  ( 4.999999999999999112, -5.222868219166923787, 9.680994141368751471 ) ) ;
#3473 = ORIENTED_EDGE ( 'NONE', *, *, #22648, .T. ) ;
#3474 = CARTESIAN_POINT ( 'NONE',  ( -66.20000000218495018, 9.999999999999998224, 17.49999999999999645 ) ) ;
#3475 = EDGE_LOOP ( 'NONE', ( #17479, #16631, #2109, #7654 ) ) ;
#3476 = EDGE_CURVE ( 'NONE', #14331, #20947, #21394, .T. ) ;
#3477 = CARTESIAN_POINT ( 'NONE',  ( 4.000000000000000888, 1.656854249492381248, 18.56250000000001421 ) ) ;
#3478 = EDGE_CURVE ( 'NONE', #22731, #313, #10811, .T. ) ;
#3479 = CARTESIAN_POINT ( 'NONE',  ( -3.999999999999998224, -1.656854249492383246, 17.06250000000001421 ) ) ;
#3480 = CARTESIAN_POINT ( 'NONE',  ( -66.44999999999998863, 8.964466094067219615, 12.50000000000003553 ) ) ;
#3481 = CIRCLE ( 'NONE', #18782, 2.500000000000002220 ) ;
#3482 = CARTESIAN_POINT ( 'NONE',  ( -3.999999999999999112, 0.000000000000000000, 11.00000000000001066 ) ) ;
#3483 = LINE ( 'NONE', #10819, #20187 ) ;
#3484 = EDGE_CURVE ( 'NONE', #2790, #15133, #20822, .T. ) ;
#3485 = DIRECTION ( 'NONE',  ( -1.000000000000000000, -0.000000000000000000, -0.000000000000000000 ) ) ;
#3486 = CARTESIAN_POINT ( 'NONE',  ( -67.49999999999998579, 12.50000000000000000, 14.99999999999999645 ) ) ;
#3487 = CARTESIAN_POINT ( 'NONE',  ( -19.99999999999999645, -9.000000000000003553, 5.000000000000079936 ) ) ;
#3488 = CARTESIAN_POINT ( 'NONE',  ( 60.00000000000001421, 11.91318284588047405, 17.59430459896656629 ) ) ;
#3489 = DIRECTION ( 'NONE',  ( -1.000000000000000000, 0.000000000000000000, 0.000000000000000000 ) ) ;
#3490 = CARTESIAN_POINT ( 'NONE',  ( -2.828427124746189403, -2.828427124746190735, 4.424999999999999822 ) ) ;
#3491 = CARTESIAN_POINT ( 'NONE',  ( -66.85000000109246798, 7.933012699999995476, 14.99999999999999645 ) ) ;
#3492 = CARTESIAN_POINT ( 'NONE',  ( -0.6948844085414769278, 3.953085111073343594, 9.999322813920281661 ) ) ;
#3493 = CARTESIAN_POINT ( 'NONE',  ( 2.445694354108821855, -2.445694354108820079, 16.81250000136560629 ) ) ;
#3494 = CARTESIAN_POINT ( 'NONE',  ( -66.35000000218495586, 7.499999999999996447, 16.03553390593273775 ) ) ;
#3495 = APPLICATION_CONTEXT ( 'automotive_design' ) ;
#3496 = VERTEX_POINT ( 'NONE', #19747 ) ;
#3497 = CARTESIAN_POINT ( 'NONE',  ( 2.828427124746191179, 2.828427124746190291, 16.75000000273119838 ) ) ;
#3498 = ORIENTED_EDGE ( 'NONE', *, *, #21456, .T. ) ;
#3499 = CARTESIAN_POINT ( 'NONE',  ( 53.31018183416157541, 14.00000000000000000, 15.06805114094561304 ) ) ;
#3500 = CARTESIAN_POINT ( 'NONE',  ( -66.35000000109248219, 11.46158073645647235, 16.46158073645647235 ) ) ;
#3501 = DIRECTION ( 'NONE',  ( 0.000000000000000000, 0.000000000000000000, -1.000000000000000000 ) ) ;
#3502 = CARTESIAN_POINT ( 'NONE',  ( 2.445694354108820523, -2.445694354108820079, -2.887499998634404097 ) ) ;
#3503 = EDGE_LOOP ( 'NONE', ( #5531, #17087, #3727, #17256 ) ) ;
#3504 = ADVANCED_FACE ( 'NONE', ( #1415 ), #12366, .F. ) ;
#3505 = ADVANCED_FACE ( 'NONE', ( #16180 ), #23469, .F. ) ;
#3506 = VERTEX_POINT ( 'NONE', #3472 ) ;
#3507 = DIRECTION ( 'NONE',  ( -0.000000000000000000, -0.000000000000000000, 1.000000000000000000 ) ) ;
#3508 = CARTESIAN_POINT ( 'NONE',  ( 54.12731816583844591, 12.16943976678978601, 17.07320092032949432 ) ) ;
#3509 = CARTESIAN_POINT ( 'NONE',  ( -70.10000000109246798, 10.85617417291294551, 12.93301269999999370 ) ) ;
#3510 = EDGE_CURVE ( 'NONE', #4668, #14091, #23589, .T. ) ;
#3511 = EDGE_CURVE ( 'NONE', #15223, #25, #12728, .T. ) ;
#3512 = CARTESIAN_POINT ( 'NONE',  ( -70.35000000109246798, 11.46158073645647235, 13.53841926354352232 ) ) ;
#3513 = CARTESIAN_POINT ( 'NONE',  ( -3.458734124999999437, 1.432654583217640498, 16.62500000136560629 ) ) ;
#3514 = DIRECTION ( 'NONE',  ( -1.000000000000000000, -0.000000000000000000, -0.000000000000000000 ) ) ;
#3515 = CARTESIAN_POINT ( 'NONE',  ( 55.50000000000000711, 12.12132034355963484, 12.87867965644034740 ) ) ;
#3516 = CARTESIAN_POINT ( 'NONE',  ( -3.999999999999999112, 0.000000000000000000, -20.00000000000000000 ) ) ;
#3517 = CARTESIAN_POINT ( 'NONE',  ( 56.15625000000002132, 7.000000000000003553, 16.24264068711929099 ) ) ;
#3518 = CARTESIAN_POINT ( 'NONE',  ( -4.000000000000000000, 0.000000000000000000, -2.699999999999999289 ) ) ;
#3519 = CARTESIAN_POINT ( 'NONE',  ( -2.247776618166699603, 3.308700692843501656, -19.99999999999999289 ) ) ;
#3520 = CARTESIAN_POINT ( 'NONE',  ( 25.24566549676620397, -9.000000000000003553, 5.000000000000079936 ) ) ;
#3521 = ORIENTED_EDGE ( 'NONE', *, *, #21761, .F. ) ;
#3522 = CARTESIAN_POINT ( 'NONE',  ( 25.00005080000000035, 5.400000000000000355, -1.000000000000000000 ) ) ;
#3523 = CARTESIAN_POINT ( 'NONE',  ( -19.99999999999999645, -9.000000000000003553, 5.000000000000079936 ) ) ;
#3524 = EDGE_LOOP ( 'NONE', ( #18220, #11976 ) ) ;
#3525 = CARTESIAN_POINT ( 'NONE',  ( 52.59375000000000711, 11.24264068711927322, 11.99999999999998934 ) ) ;
#3526 = CARTESIAN_POINT ( 'NONE',  ( -4.000000000000000888, 1.656854249492380804, -2.637499997268812013 ) ) ;
#3527 = CARTESIAN_POINT ( 'NONE',  ( 4.999999999999999112, -8.152713396088739017, -3.174628368996162298 ) ) ;
#3528 = VERTEX_POINT ( 'NONE', #1192 ) ;
#3529 = CARTESIAN_POINT ( 'NONE',  ( 4.000000000000000888, 4.898587196589412829E-16, 16.50000000000001066 ) ) ;
#3530 = ORIENTED_EDGE ( 'NONE', *, *, #6636, .T. ) ;
#3531 = CARTESIAN_POINT ( 'NONE',  ( 0.000000000000000000, 8.264486777890107660, -4.472189673936815879 ) ) ;
#3532 = EDGE_CURVE ( 'NONE', #15758, #14307, #13162, .T. ) ;
#3533 = CARTESIAN_POINT ( 'NONE',  ( 4.000000000000000000, 4.898587196589412829E-16, 0.8000000000000020428 ) ) ;
#3534 = ORIENTED_EDGE ( 'NONE', *, *, #10135, .F. ) ;
#3535 = CARTESIAN_POINT ( 'NONE',  ( 2.499999999999999556, 7.593217523260696211, -7.958834565716683684 ) ) ;
#3536 = ORIENTED_EDGE ( 'NONE', *, *, #3784, .F. ) ;
#3537 = LINE ( 'NONE', #21605, #5643 ) ;
#3538 = EDGE_CURVE ( 'NONE', #10786, #10158, #16412, .T. ) ;
#3539 = CARTESIAN_POINT ( 'NONE',  ( 65.85000000109246798, 9.999999999999998224, 17.06698730000000097 ) ) ;
#3540 = CARTESIAN_POINT ( 'NONE',  ( -2.974182810908594821, 5.788408252967899514, -3.700000000000004174 ) ) ;
#3541 = CARTESIAN_POINT ( 'NONE',  ( -20.00005079999999680, 0.000000000000000000, 0.000000000000000000 ) ) ;
#3542 = CARTESIAN_POINT ( 'NONE',  ( 55.81481816583843170, 14.00000000000000178, 14.93194885905434610 ) ) ;
#3543 = CARTESIAN_POINT ( 'NONE',  ( -1.432654583217640942, -3.458734124999999882, -1.074999998634403209 ) ) ;
#3544 = CARTESIAN_POINT ( 'NONE',  ( -3.458734124999998993, 0.000000000000000000, 12.43750000136560629 ) ) ;
#3545 = DIRECTION ( 'NONE',  ( 1.000000000000000000, 0.000000000000000000, 0.000000000000000000 ) ) ;
#3546 = DIRECTION ( 'NONE',  ( -1.000000000000000000, 0.000000000000000000, 0.000000000000000000 ) ) ;
#3547 = VERTEX_POINT ( 'NONE', #7788 ) ;
#3548 = CARTESIAN_POINT ( 'NONE',  ( 6.499999999999999112, -3.752776749732574135, -3.119443416399232394 ) ) ;
#3549 = LINE ( 'NONE', #5228, #2514 ) ;
#3550 = CARTESIAN_POINT ( 'NONE',  ( 72.50000000000000000, 9.999999999999998224, 14.99999999999999645 ) ) ;
#3551 = ORIENTED_EDGE ( 'NONE', *, *, #1434, .F. ) ;
#3552 = ORIENTED_EDGE ( 'NONE', *, *, #7740, .T. ) ;
#3553 = CARTESIAN_POINT ( 'NONE',  ( -4.000000000000000000, 0.000000000000000000, -1.574999997268811569 ) ) ;
#3554 = CARTESIAN_POINT ( 'NONE',  ( 58.87500000000000711, 7.171572875253794166, 12.17157287525381726 ) ) ;
#3555 = ORIENTED_EDGE ( 'NONE', *, *, #14408, .T. ) ;
#3556 = CARTESIAN_POINT ( 'NONE',  ( 2.500000000000000000, 2.500728763858895382E-16, -2.041999999999999815 ) ) ;
#3557 = EDGE_LOOP ( 'NONE', ( #3991, #655 ) ) ;
#3558 = AXIS2_PLACEMENT_3D ( 'NONE', #20770, #11712, #9456 ) ;
#3559 = CARTESIAN_POINT ( 'NONE',  ( 51.37500000000000711, 7.171572875253794166, 12.17157287525381726 ) ) ;
#3560 = VECTOR ( 'NONE', #2862, 1000.000000000000000 ) ;
#3561 = ADVANCED_FACE ( 'NONE', ( #7547, #10918 ), #11268, .T. ) ;
#3562 = CARTESIAN_POINT ( 'NONE',  ( 66.40000000218495302, 7.499999999999996447, 14.99999999999999645 ) ) ;
#3563 = CARTESIAN_POINT ( 'NONE',  ( 72.50000000000000000, 9.999999999999998224, 14.99999999999999645 ) ) ;
#3564 = LINE ( 'NONE', #5481, #6043 ) ;
#3565 = CARTESIAN_POINT ( 'NONE',  ( -13.27237933033274153, -11.25000000000000355, 5.000000000000079936 ) ) ;
#3566 = ORIENTED_EDGE ( 'NONE', *, *, #15515, .T. ) ;
#3567 = CARTESIAN_POINT ( 'NONE',  ( -3.999999999999998224, -1.656854249492383246, 18.18750000273119483 ) ) ;
#3568 = DIRECTION ( 'NONE',  ( 1.000000000000000000, 0.000000000000000000, 0.000000000000000000 ) ) ;
#3569 = CARTESIAN_POINT ( 'NONE',  ( 59.40393183416158251, 14.02818770551463956, 13.41119689145323335 ) ) ;
#3570 = DIRECTION ( 'NONE',  ( 1.000000000000000000, -0.000000000000000000, -0.000000000000000000 ) ) ;
#3571 = CARTESIAN_POINT ( 'NONE',  ( 66.40000000109247935, 12.06698730000000275, 14.14382582708705094 ) ) ;
#3572 = DIRECTION ( 'NONE',  ( -1.000000000000000000, 0.000000000000000000, 0.000000000000000000 ) ) ;
#3573 = AXIS2_PLACEMENT_3D ( 'NONE', #1965, #60, #19939 ) ;
#3574 = DIRECTION ( 'NONE',  ( 0.000000000000000000, 0.3090169943749412895, 0.9510565162951555296 ) ) ;
#3575 = VERTEX_POINT ( 'NONE', #4056 ) ;
#3576 = CARTESIAN_POINT ( 'NONE',  ( -3.729367062499998831, 0.000000000000000000, 19.84375000068280670 ) ) ;
#3577 = CARTESIAN_POINT ( 'NONE',  ( 58.68750000000000000, 9.999999999999989342, 11.99999999999999467 ) ) ;
#3578 = CARTESIAN_POINT ( 'NONE',  ( -4.714285714285714413, 5.773334910266094008E-16, 2.039999999999998259 ) ) ;
#3579 = SHAPE_REPRESENTATION_RELATIONSHIP ( 'NONE' , 'NONE' ,  #9307, #19874 ) ;
#3580 = EDGE_LOOP ( 'NONE', ( #1191, #13275, #5824, #223 ) ) ;
#3581 = FACE_OUTER_BOUND ( 'NONE', #6661, .T. ) ;
#3582 = CARTESIAN_POINT ( 'NONE',  ( -2.117863837641485618E-16, 3.458734125000000326, -2.512499998634404097 ) ) ;
#3583 = CARTESIAN_POINT ( 'NONE',  ( -19.55556463033274284, -11.25000000000000355, 5.000000000000079936 ) ) ;
#3584 = ORIENTED_EDGE ( 'NONE', *, *, #9637, .T. ) ;
#3585 = CARTESIAN_POINT ( 'NONE',  ( 69.84999999999999432, 12.50000000000000000, 13.96446609406725692 ) ) ;
#3586 = VERTEX_POINT ( 'NONE', #12833 ) ;
#3587 = DIRECTION ( 'NONE',  ( -1.224646799147353207E-16, 0.000000000000000000, -1.000000000000000000 ) ) ;
#3588 = CARTESIAN_POINT ( 'NONE',  ( 1.656854249492384135, -3.999999999999999112, 18.31250000000001421 ) ) ;
#3589 = LINE ( 'NONE', #21899, #774 ) ;
#3590 = CARTESIAN_POINT ( 'NONE',  ( -67.85000000218494165, 8.964466094067287116, 17.50000000000002487 ) ) ;
#3591 = CARTESIAN_POINT ( 'NONE',  ( -19.99999999999999645, -9.000000000000003553, 10.00000000000008882 ) ) ;
#3592 = FACE_OUTER_BOUND ( 'NONE', #6776, .T. ) ;
#3593 = CARTESIAN_POINT ( 'NONE',  ( -67.09999999999999432, 7.499999999999996447, 14.99999999999999645 ) ) ;
#3594 = CYLINDRICAL_SURFACE ( 'NONE', #4943, 4.000000000000000000 ) ;
#3595 = CARTESIAN_POINT ( 'NONE',  ( -1.432654583217639610, -3.458734124999999882, 16.62500000136560629 ) ) ;
#3596 = CARTESIAN_POINT ( 'NONE',  ( -6.259644161404860030E-16, -4.618802153517027165, -3.433295621305388234 ) ) ;
#3597 = EDGE_CURVE ( 'NONE', #18669, #8348, #11310, .T. ) ;
#3598 = CARTESIAN_POINT ( 'NONE',  ( 4.000000000000000000, 4.898587196589412829E-16, 3.800000000000002931 ) ) ;
#3599 = DIRECTION ( 'NONE',  ( -1.000000000000000000, -0.000000000000000000, -0.000000000000000000 ) ) ;
#3600 = CARTESIAN_POINT ( 'NONE',  ( -2.445694354108818303, -2.445694354108820523, 15.56250000136560629 ) ) ;
#3601 = CARTESIAN_POINT ( 'NONE',  ( -66.25000000218494733, 8.964466094067207180, 17.49999999999995026 ) ) ;
#3602 = ORIENTED_EDGE ( 'NONE', *, *, #11998, .F. ) ;
#3603 = CARTESIAN_POINT ( 'NONE',  ( -69.85000000109248219, 7.933012699999995476, 14.99999999999999645 ) ) ;
#3604 = EDGE_LOOP ( 'NONE', ( #1577, #4463, #18161, #11524 ) ) ;
#3605 = CARTESIAN_POINT ( 'NONE',  ( 52.46643183416157541, 6.028187705514633343, 13.27509460956200016 ) ) ;
#3606 = CARTESIAN_POINT ( 'NONE',  ( -66.50000000109247367, 9.143825827087049163, 17.06698729999999742 ) ) ;
#3607 = CARTESIAN_POINT ( 'NONE',  ( 70.00000000000000000, 10.00000000000000000, 14.99999999999999645 ) ) ;
#3608 = EDGE_CURVE ( 'NONE', #12123, #2153, #20444, .T. ) ;
#3609 = DIRECTION ( 'NONE',  ( 1.000000000000000000, 0.000000000000000000, -1.224646799147353207E-16 ) ) ;
#3610 = VERTEX_POINT ( 'NONE', #11387 ) ;
#3611 = EDGE_LOOP ( 'NONE', ( #1388, #11614, #16915 ) ) ;
#3612 = DIRECTION ( 'NONE',  ( -0.000000000000000000, -0.000000000000000000, 1.000000000000000000 ) ) ;
#3613 = CARTESIAN_POINT ( 'NONE',  ( 53.09606816583843170, 11.17458954617364242, 11.97181229448534800 ) ) ;
#3614 = VECTOR ( 'NONE', #23283, 1000.000000000000000 ) ;
#3615 = CARTESIAN_POINT ( 'NONE',  ( -65.65000000218493881, 7.499999999999995559, 13.96446609406725692 ) ) ;
#3616 = AXIS2_PLACEMENT_3D ( 'NONE', #20348, #19888, #3489 ) ;
#3617 = CARTESIAN_POINT ( 'NONE',  ( -68.95000000109247651, 11.46158073645647235, 16.46158073645647235 ) ) ;
#3618 = CARTESIAN_POINT ( 'NONE',  ( -1.432654583217639832, -3.458734125000000326, 10.87500000136560452 ) ) ;
#3619 = CARTESIAN_POINT ( 'NONE',  ( 1.971781867644420635E-15, -4.000000000000000000, 10.37500000273119660 ) ) ;
#3620 = CARTESIAN_POINT ( 'NONE',  ( 53.15625000000001421, 7.000000000000003553, 16.24264068711929099 ) ) ;
#3621 = DIRECTION ( 'NONE',  ( -1.000000000000000000, 0.000000000000000000, 0.000000000000000000 ) ) ;
#3622 = ADVANCED_FACE ( 'NONE', ( #22362 ), #17419, .T. ) ;
#3623 = CARTESIAN_POINT ( 'NONE',  ( 52.12500000000000711, 12.12132034355964727, 17.12132034355963484 ) ) ;
#3624 = ADVANCED_FACE ( 'NONE', ( #13300 ), #16638, .F. ) ;
#3625 = CARTESIAN_POINT ( 'NONE',  ( 2.000000000000001776, 1.089935651241147118E-15, 8.800000000000023803 ) ) ;
#3626 = CARTESIAN_POINT ( 'NONE',  ( -68.49999999999998579, 9.999999999999998224, 17.49999999999999645 ) ) ;
#3627 = EDGE_LOOP ( 'NONE', ( #6368, #3964, #20949 ) ) ;
#3628 = DIRECTION ( 'NONE',  ( 1.000000000000000000, 0.000000000000000000, 0.000000000000000000 ) ) ;
#3629 = DIRECTION ( 'NONE',  ( 1.000000000000000000, 0.000000000000000000, 0.000000000000000000 ) ) ;
#3630 = VERTEX_POINT ( 'NONE', #219 ) ;
#3631 = CARTESIAN_POINT ( 'NONE',  ( 54.46875000000000000, 6.999999999999992895, 13.75735931288071967 ) ) ;
#3632 = AXIS2_PLACEMENT_3D ( 'NONE', #18028, #10754, #16350 ) ;
#3633 = CARTESIAN_POINT ( 'NONE',  ( -2.445694354108819635, -2.445694354108820523, 4.862500001365595459 ) ) ;
#3634 = VECTOR ( 'NONE', #7399, 1000.000000000000000 ) ;
#3635 = EDGE_CURVE ( 'NONE', #19193, #23445, #5976, .T. ) ;
#3636 = CYLINDRICAL_SURFACE ( 'NONE', #12079, 2.500000000000000444 ) ;
#3637 = ORIENTED_EDGE ( 'NONE', *, *, #8976, .T. ) ;
#3638 = CARTESIAN_POINT ( 'NONE',  ( 4.000000000000001776, -1.656854249492379694, 16.43750000000001066 ) ) ;
#3639 = CARTESIAN_POINT ( 'NONE',  ( -2.449293598294706907E-16, 4.000000000000000000, -2.949999999999997957 ) ) ;
#3640 = DIRECTION ( 'NONE',  ( -7.087422195345011518E-32, -1.000000000000000000, -0.000000000000000000 ) ) ;
#3641 = ORIENTED_EDGE ( 'NONE', *, *, #2865, .T. ) ;
#3642 = DIRECTION ( 'NONE',  ( 0.000000000000000000, 0.000000000000000000, 1.000000000000000000 ) ) ;
#3643 = LINE ( 'NONE', #5568, #9093 ) ;
#3644 = CARTESIAN_POINT ( 'NONE',  ( 4.999999999999999112, 6.478011392632982535, -6.807171995660517005 ) ) ;
#3645 = AXIS2_PLACEMENT_3D ( 'NONE', #22187, #3878, #49 ) ;
#3646 = CARTESIAN_POINT ( 'NONE',  ( 72.44999999999998863, 11.03553390593273598, 17.50000000000000355 ) ) ;
#3647 = ADVANCED_FACE ( 'NONE', ( #18317 ), #3693, .T. ) ;
#3648 = CIRCLE ( 'NONE', #17439, 11.00000000000000000 ) ;
#3649 = CARTESIAN_POINT ( 'NONE',  ( 1.567478505476134606E-15, 4.618802153517012066, -5.000000000000000000 ) ) ;
#3650 = LINE ( 'NONE', #1850, #21769 ) ;
#3651 = CARTESIAN_POINT ( 'NONE',  ( 51.78356816583844591, 8.275094609561968184, 11.02818770551464667 ) ) ;
#3652 = EDGE_CURVE ( 'NONE', #7101, #9090, #22392, .T. ) ;
#3653 = CARTESIAN_POINT ( 'NONE',  ( -1.432654583217640276, 3.458734125000000326, -0.4499999986344046521 ) ) ;
#3654 = CARTESIAN_POINT ( 'NONE',  ( -2.413812496766188698, -9.000000000000003553, 5.000000000000079936 ) ) ;
#3655 = CARTESIAN_POINT ( 'NONE',  ( -3.999999999999999112, 0.000000000000000000, 18.12500000273119483 ) ) ;
#3656 = AXIS2_PLACEMENT_3D ( 'NONE', #21284, #10210, #2511 ) ;
#3657 = DIRECTION ( 'NONE',  ( 0.000000000000000000, 0.000000000000000000, 1.000000000000000000 ) ) ;
#3658 = ORIENTED_EDGE ( 'NONE', *, *, #5258, .T. ) ;
#3659 = DIRECTION ( 'NONE',  ( 0.000000000000000000, -0.000000000000000000, 1.000000000000000000 ) ) ;
#3660 = CARTESIAN_POINT ( 'NONE',  ( 4.999999999999999112, 0.000000000000000000, 0.000000000000000000 ) ) ;
#3661 = DIRECTION ( 'NONE',  ( 0.000000000000000000, 0.000000000000000000, 1.000000000000000000 ) ) ;
#3662 = EDGE_CURVE ( 'NONE', #22700, #7989, #4277, .T. ) ;
#3663 = ORIENTED_EDGE ( 'NONE', *, *, #1140, .F. ) ;
#3664 = EDGE_CURVE ( 'NONE', #4715, #21630, #9242, .T. ) ;
#3665 = ORIENTED_EDGE ( 'NONE', *, *, #9394, .T. ) ;
#3666 = CARTESIAN_POINT ( 'NONE',  ( 20.00000000000000000, 1.500000000000003109, -17.32050807568893092 ) ) ;
#3667 = CARTESIAN_POINT ( 'NONE',  ( 54.00000000000000711, 12.82842712474617741, 12.17157287525379239 ) ) ;
#3668 = ORIENTED_EDGE ( 'NONE', *, *, #18149, .T. ) ;
#3669 = CARTESIAN_POINT ( 'NONE',  ( -5.564649990716551642, -8.974600000000002353, 5.000000000000079936 ) ) ;
#3670 = VERTEX_POINT ( 'NONE', #16761 ) ;
#3671 = CARTESIAN_POINT ( 'NONE',  ( 51.97106816583844591, 5.971812294485345340, 13.41119689145326710 ) ) ;
#3672 = CARTESIAN_POINT ( 'NONE',  ( 65.60000000218495586, 7.499999999999996447, 14.99999999999999645 ) ) ;
#3673 = DIRECTION ( 'NONE',  ( 0.000000000000000000, 0.000000000000000000, -1.000000000000000000 ) ) ;
#3674 = DIRECTION ( 'NONE',  ( -1.000000000000000000, 0.000000000000000000, 0.000000000000000000 ) ) ;
#3675 = CARTESIAN_POINT ( 'NONE',  ( -1.656854249492381248, -3.999999999999999112, -0.5124999999999968470 ) ) ;
#3676 = ORIENTED_EDGE ( 'NONE', *, *, #13932, .F. ) ;
#3677 = CARTESIAN_POINT ( 'NONE',  ( 1.656854249492381470, 4.000000000000000000, 18.81250000273119838 ) ) ;
#3678 = CARTESIAN_POINT ( 'NONE',  ( -2.117863837641485618E-16, 3.458734125000000770, -3.262499998634402765 ) ) ;
#3679 = CARTESIAN_POINT ( 'NONE',  ( 52.37268183416157541, 7.219692298483935566, 12.12345345202367675 ) ) ;
#3680 = CARTESIAN_POINT ( 'NONE',  ( 1.125461230421587633, -3.270501301980698550, 2.040000000000001812 ) ) ;
#3681 = FACE_OUTER_BOUND ( 'NONE', #5611, .T. ) ;
#3682 = CARTESIAN_POINT ( 'NONE',  ( -20.00000000000000711, 1.500000000000003109, -17.32050807568893092 ) ) ;
#3683 = CARTESIAN_POINT ( 'NONE',  ( 45.00000000000000000, 10.00000000000001599, 34.11836509645781490 ) ) ;
#3684 = ORIENTED_EDGE ( 'NONE', *, *, #19014, .F. ) ;
#3685 = DIRECTION ( 'NONE',  ( -1.000000000000000000, 0.000000000000000000, 0.000000000000000000 ) ) ;
#3686 = CARTESIAN_POINT ( 'NONE',  ( 51.46875000000000711, 6.999999999999992006, 13.75735931288071967 ) ) ;
#3687 = FACE_OUTER_BOUND ( 'NONE', #17622, .T. ) ;
#3688 = EDGE_CURVE ( 'NONE', #11955, #2020, #16528, .T. ) ;
#3689 = EDGE_CURVE ( 'NONE', #23683, #8317, #6280, .T. ) ;
#3690 = ORIENTED_EDGE ( 'NONE', *, *, #6931, .F. ) ;
#3691 = CARTESIAN_POINT ( 'NONE',  ( -4.000000000000000000, 2.309401076758498483, -3.433295621305379353 ) ) ;
#3692 = CARTESIAN_POINT ( 'NONE',  ( -3.458734124999999882, -1.432654583217642497, -3.199999998634404985 ) ) ;
#3693 = PLANE ( 'NONE',  #8269 ) ;
#3694 = ORIENTED_EDGE ( 'NONE', *, *, #5667, .T. ) ;
#3695 = DIRECTION ( 'NONE',  ( -0.3420201433256622181, 0.9396926207859106484, 1.232595164407828100E-31 ) ) ;
#3696 = ORIENTED_EDGE ( 'NONE', *, *, #524, .T. ) ;
#3697 = CARTESIAN_POINT ( 'NONE',  ( -3.999999999999999112, 0.000000000000000000, 19.12500000273119838 ) ) ;
#3698 = AXIS2_PLACEMENT_3D ( 'NONE', #5075, #1704, #12297 ) ;
#3699 = CARTESIAN_POINT ( 'NONE',  ( -2.445694354108819191, 2.445694354108820523, 10.56250000136560629 ) ) ;
#3700 = CARTESIAN_POINT ( 'NONE',  ( 2.499999999999999556, 7.958834565716877307, -7.593217523260497259 ) ) ;
#3701 = DIRECTION ( 'NONE',  ( -0.3420201433256622181, 0.9396926207859106484, 1.232595164407828100E-31 ) ) ;
#3702 = CYLINDRICAL_SURFACE ( 'NONE', #12971, 4.000000000000000000 ) ;
#3703 = ORIENTED_EDGE ( 'NONE', *, *, #11123, .F. ) ;
#3704 = VECTOR ( 'NONE', #1044, 1000.000000000000000 ) ;
#3705 = CIRCLE ( 'NONE', #4093, 11.00000000000000000 ) ;
#3706 = DIRECTION ( 'NONE',  ( 0.000000000000000000, 0.000000000000000000, 1.000000000000000000 ) ) ;
#3707 = CARTESIAN_POINT ( 'NONE',  ( 3.250000000000004441, 5.629165124598849879, -3.700000000000000178 ) ) ;
#3708 = CARTESIAN_POINT ( 'NONE',  ( 66.70000000109246230, 7.933012699999995476, 14.14382582708705094 ) ) ;
#3709 = CARTESIAN_POINT ( 'NONE',  ( -2.445694354108819191, 2.445694354108820523, 18.31250000136560274 ) ) ;
#3710 = DIRECTION ( 'NONE',  ( 0.000000000000000000, 0.000000000000000000, 1.000000000000000000 ) ) ;
#3711 = CARTESIAN_POINT ( 'NONE',  ( -2.117863837641485618E-16, 3.458734125000000770, -2.262499998634403653 ) ) ;
#3712 = CARTESIAN_POINT ( 'NONE',  ( 43.27628836966725601, -11.25000000000000355, 10.00000000000008882 ) ) ;
#3713 = CARTESIAN_POINT ( 'NONE',  ( 1.025207404391860050E-15, 3.458734125000000326, 15.18750000136560452 ) ) ;
#3714 = CARTESIAN_POINT ( 'NONE',  ( -90.00000000000000000, 7.347880794884145374E-16, 6.000000000000021316 ) ) ;
#3715 = ORIENTED_EDGE ( 'NONE', *, *, #10558, .F. ) ;
#3716 = AXIS2_PLACEMENT_3D ( 'NONE', #15586, #6225, #17250 ) ;
#3717 = CARTESIAN_POINT ( 'NONE',  ( -68.80000000109247082, 10.85617417291294551, 17.06698730000000097 ) ) ;
#3718 = VERTEX_POINT ( 'NONE', #691 ) ;
#3719 = CARTESIAN_POINT ( 'NONE',  ( 57.43518183416157541, 9.931948859054379852, 18.99999999999999289 ) ) ;
#3720 = CARTESIAN_POINT ( 'NONE',  ( -72.05000000109245661, 12.06698730000000097, 14.99999999999999645 ) ) ;
#3721 = ITEM_DEFINED_TRANSFORMATION ( 'NONE', 'NONE', #6066,  #7318 ) ;
#3722 = CARTESIAN_POINT ( 'NONE',  ( -4.000000000000000888, 1.656854249492380582, 1.362500002731187321 ) ) ;
#3723 = ORIENTED_EDGE ( 'NONE', *, *, #13353, .F. ) ;
#3724 = VECTOR ( 'NONE', #8124, 1000.000000000000000 ) ;
#3725 = AXIS2_PLACEMENT_3D ( 'NONE', #12394, #18668, #19659 ) ;
#3726 = PRODUCT_DEFINITION ( 'UNKNOWN', '', #11848, #923 ) ;
#3727 = ORIENTED_EDGE ( 'NONE', *, *, #3766, .T. ) ;
#3728 = CARTESIAN_POINT ( 'NONE',  ( 7.000000000000000000, 0.000000000000000000, 1.734723475976807094E-15 ) ) ;
#3729 = CARTESIAN_POINT ( 'NONE',  ( 54.22106816583844591, 13.02818770551464489, 16.17458954617363531 ) ) ;
#3730 = EDGE_CURVE ( 'NONE', #18141, #2469, #1742, .T. ) ;
#3731 = CARTESIAN_POINT ( 'NONE',  ( -71.25000000109248788, 9.999999999999998224, 17.06698730000000097 ) ) ;
#3732 = VECTOR ( 'NONE', #9098, 1000.000000000000000 ) ;
#3733 = CARTESIAN_POINT ( 'NONE',  ( -70.60000000109246798, 10.85617417291294551, 17.06698729999999742 ) ) ;
#3734 = CARTESIAN_POINT ( 'NONE',  ( 1.432654583217641386, 3.458734125000000770, 12.37500000136560629 ) ) ;
#3735 = DIRECTION ( 'NONE',  ( 0.8660254037844383745, 0.5000000000000004441, 0.000000000000000000 ) ) ;
#3736 = CARTESIAN_POINT ( 'NONE',  ( 51.18750000000000711, 9.999999999999989342, 11.99999999999999467 ) ) ;
#3737 = CARTESIAN_POINT ( 'NONE',  ( 0.000000000000000000, -4.057423117305329896, -8.475820894093020641 ) ) ;
#3738 = VECTOR ( 'NONE', #12191, 1000.000000000000000 ) ;
#3739 = AXIS2_PLACEMENT_3D ( 'NONE', #4245, #19201, #2545 ) ;
#3740 = CARTESIAN_POINT ( 'NONE',  ( 53.62500000000000711, 12.12132034355964727, 17.12132034355963484 ) ) ;
#3741 = CARTESIAN_POINT ( 'NONE',  ( 4.000000000000001776, -1.656854249492379694, 14.56250000273119660 ) ) ;
#3742 = CARTESIAN_POINT ( 'NONE',  ( 37.81203609676620658, -9.000000000000005329, 10.00000000000008882 ) ) ;
#3743 = VERTEX_POINT ( 'NONE', #4650 ) ;
#3744 = FACE_OUTER_BOUND ( 'NONE', #20065, .T. ) ;
#3745 = DIRECTION ( 'NONE',  ( 0.000000000000000000, -0.4999999999999993339, 0.8660254037844390407 ) ) ;
#3746 = ORIENTED_EDGE ( 'NONE', *, *, #18358, .T. ) ;
#3747 = CARTESIAN_POINT ( 'NONE',  ( 53.34375000000000000, 8.757359312880723223, 18.00000000000000355 ) ) ;
#3748 = CARTESIAN_POINT ( 'NONE',  ( -3.458734124999999882, -1.432654583217642497, 4.800000001365595459 ) ) ;
#3749 = CARTESIAN_POINT ( 'NONE',  ( -6.500000000000000000, -3.752776749732573247, -0.5805565836007695601 ) ) ;
#3750 = VERTEX_POINT ( 'NONE', #20914 ) ;
#3751 = CARTESIAN_POINT ( 'NONE',  ( 2.828427124746192067, -2.828427124746189847, 15.37500000000001066 ) ) ;
#3752 = AXIS2_PLACEMENT_3D ( 'NONE', #14729, #18295, #19609 ) ;
#3753 = CARTESIAN_POINT ( 'NONE',  ( -1.600000000000004086, 0.000000000000000000, 0.000000000000000000 ) ) ;
#3754 =( BOUNDED_CURVE ( )  B_SPLINE_CURVE ( 2, ( #22445, #15069, #22326, #5940, #13266, #2339, #4490, #21002, #15544 ),
 .UNSPECIFIED., .F., .F. ) 
 B_SPLINE_CURVE_WITH_KNOTS ( ( 3, 2, 2, 2, 3 ),
 ( 0.3749999999999998890, 0.3906249999999997780, 0.4062499999999996669, 0.4218749999999996114, 0.4374999999999995004 ),
 .UNSPECIFIED. ) 
 CURVE ( )  GEOMETRIC_REPRESENTATION_ITEM ( )  RATIONAL_B_SPLINE_CURVE ( ( 1.000000000000000444, 0.9238795325112861834, 1.000000000000000000, 0.9238795325112867385, 1.000000000000000000, 0.9238795325112867385, 1.000000000000000000, 0.9238795325112891810, 0.9999999999999975575 ) ) 
 REPRESENTATION_ITEM ( '' )  );
#3755 = DIRECTION ( 'NONE',  ( 0.000000000000000000, 0.000000000000000000, 1.000000000000000000 ) ) ;
#3756 = VERTEX_POINT ( 'NONE', #573 ) ;
#3757 = LINE ( 'NONE', #19815, #14156 ) ;
#3758 = PRODUCT_DEFINITION_SHAPE ( 'NONE', 'NONE',  #520 ) ;
#3759 = EDGE_CURVE ( 'NONE', #19804, #10717, #10194, .T. ) ;
#3760 = CIRCLE ( 'NONE', #23268, 2.649999999999989253 ) ;
#3761 = CARTESIAN_POINT ( 'NONE',  ( 18.97172504071656363, -8.974600000000002353, 10.00000000000008882 ) ) ;
#3762 = EDGE_CURVE ( 'NONE', #20778, #3988, #5185, .T. ) ;
#3763 = CARTESIAN_POINT ( 'NONE',  ( -1.432654583217640498, 3.458734125000000770, 0.8000000013655964581 ) ) ;
#3764 = CARTESIAN_POINT ( 'NONE',  ( 69.29999999999999716, 9.999999999999998224, 17.49999999999999645 ) ) ;
#3765 = AXIS2_PLACEMENT_3D ( 'NONE', #9479, #20344, #478 ) ;
#3766 = EDGE_CURVE ( 'NONE', #11384, #299, #2485, .T. ) ;
#3767 = DIRECTION ( 'NONE',  ( 0.000000000000000000, 5.754033390038004481E-16, -1.000000000000000000 ) ) ;
#3768 = CIRCLE ( 'NONE', #9926, 8.749000000000002331 ) ;
#3769 = LINE ( 'NONE', #15301, #16820 ) ;
#3770 = CARTESIAN_POINT ( 'NONE',  ( 52.06481816583844591, 5.999999999999996447, 15.06805114094564502 ) ) ;
#3771 = CARTESIAN_POINT ( 'NONE',  ( -2.117863837641485618E-16, 3.458734125000000326, 1.487500001365596125 ) ) ;
#3772 = CARTESIAN_POINT ( 'NONE',  ( -3.458734124999999437, 0.000000000000000000, 14.68750000136560452 ) ) ;
#3773 = FACE_OUTER_BOUND ( 'NONE', #22154, .T. ) ;
#3774 = CARTESIAN_POINT ( 'NONE',  ( 4.999999999999999112, -3.174628368996134320, 8.152713396088753228 ) ) ;
#3775 = ORIENTED_EDGE ( 'NONE', *, *, #1173, .T. ) ;
#3776 = CARTESIAN_POINT ( 'NONE',  ( 19.99999999999999645, 1.500000000000003109, -50.00000000000000000 ) ) ;
#3777 = AXIS2_PLACEMENT_3D ( 'NONE', #2933, #4630, #8587 ) ;
#3778 = DIRECTION ( 'NONE',  ( 0.3420201433256622736, 0.9396926207859106484, 0.000000000000000000 ) ) ;
#3779 = DIRECTION ( 'NONE',  ( 7.087422195345011518E-32, 1.000000000000000000, -0.000000000000000000 ) ) ;
#3780 = ORIENTED_EDGE ( 'NONE', *, *, #2231, .F. ) ;
#3781 = ORIENTED_EDGE ( 'NONE', *, *, #2914, .F. ) ;
#3782 = FACE_OUTER_BOUND ( 'NONE', #15118, .T. ) ;
#3783 = AXIS2_PLACEMENT_3D ( 'NONE', #12449, #17597, #19598 ) ;
#3784 = EDGE_CURVE ( 'NONE', #11205, #15638, #19338, .T. ) ;
#3785 = VERTEX_POINT ( 'NONE', #6338 ) ;
#3786 = VECTOR ( 'NONE', #8893, 1000.000000000000000 ) ;
#3787 = CARTESIAN_POINT ( 'NONE',  ( 58.12500000000000000, 12.82842712474620228, 17.82842712474617386 ) ) ;
#3788 = ORIENTED_EDGE ( 'NONE', *, *, #2005, .F. ) ;
#3789 = DIRECTION ( 'NONE',  ( 0.000000000000000000, 0.000000000000000000, -1.000000000000000000 ) ) ;
#3790 = EDGE_LOOP ( 'NONE', ( #901, #7731, #8155, #9710 ) ) ;
#3791 = AXIS2_PLACEMENT_3D ( 'NONE', #1882, #19730, #16396 ) ;
#3792 = CARTESIAN_POINT ( 'NONE',  ( 55.15856816583844591, 6.028187705514649330, 16.72490539043803182 ) ) ;
#3793 = EDGE_CURVE ( 'NONE', #10478, #5522, #10414, .T. ) ;
#3794 = EDGE_CURVE ( 'NONE', #3455, #19485, #17452, .T. ) ;
#3795 = CARTESIAN_POINT ( 'NONE',  ( 70.55000000109247082, 8.538419263543522320, 16.46158073645647235 ) ) ;
#3796 = PRODUCT_DEFINITION_FORMATION_WITH_SPECIFIED_SOURCE ( 'ANY', '', #12046, .NOT_KNOWN. ) ;
#3797 =( GEOMETRIC_REPRESENTATION_CONTEXT ( 3 ) GLOBAL_UNCERTAINTY_ASSIGNED_CONTEXT ( ( #17687 ) ) GLOBAL_UNIT_ASSIGNED_CONTEXT ( ( #19455, #6773, #14089 ) ) REPRESENTATION_CONTEXT ( 'NONE', 'WORKASPACE' ) );
#3798 = DIRECTION ( 'NONE',  ( 0.000000000000000000, 0.000000000000000000, -1.000000000000000000 ) ) ;
#3799 = CARTESIAN_POINT ( 'NONE',  ( 71.00000000109245946, 9.143825827087050939, 12.93301269999999370 ) ) ;
#3800 = ADVANCED_FACE ( 'NONE', ( #22968 ), #814, .T. ) ;
#3801 = VERTEX_POINT ( 'NONE', #1045 ) ;
#3802 = CARTESIAN_POINT ( 'NONE',  ( -1.656854249492380138, -3.999999999999999112, 18.31250000273119838 ) ) ;
#3803 = EDGE_CURVE ( 'NONE', #14363, #19081, #18792, .T. ) ;
#3804 = APPLICATION_CONTEXT ( 'automotive_design' ) ;
#3805 = DIRECTION ( 'NONE',  ( 0.000000000000000000, 0.000000000000000000, -1.000000000000000000 ) ) ;
#3806 = CARTESIAN_POINT ( 'NONE',  ( 60.00000000000000711, 12.82842712474617741, 12.17157287525379239 ) ) ;
#3807 = FACE_OUTER_BOUND ( 'NONE', #18821, .T. ) ;
#3808 = AXIS2_PLACEMENT_3D ( 'NONE', #3452, #17945, #14727 ) ;
#3809 = CARTESIAN_POINT ( 'NONE',  ( 4.999999999999999112, -6.807171995660630692, 6.478011392632865295 ) ) ;
#3810 = CARTESIAN_POINT ( 'NONE',  ( 72.20000000000000284, 11.76776695296636888, 13.23223304703362579 ) ) ;
#3811 = AXIS2_PLACEMENT_3D ( 'NONE', #21020, #8133, #15444 ) ;
#3812 = FACE_OUTER_BOUND ( 'NONE', #21687, .T. ) ;
#3813 = ORIENTED_EDGE ( 'NONE', *, *, #17425, .F. ) ;
#3814 = CARTESIAN_POINT ( 'NONE',  ( -70.20000000218495018, 9.999999999999998224, 17.49999999999999645 ) ) ;
#3815 = CARTESIAN_POINT ( 'NONE',  ( 51.37500000000000711, 7.878679656440349177, 12.87867965644035984 ) ) ;
#3816 = DIRECTION ( 'NONE',  ( 0.000000000000000000, 0.000000000000000000, 1.000000000000000000 ) ) ;
#3817 = FILL_AREA_STYLE_COLOUR ( '', #405 ) ;
#3818 = AXIS2_PLACEMENT_3D ( 'NONE', #10655, #12092, #23434 ) ;
#3819 = ORIENTED_EDGE ( 'NONE', *, *, #14346, .T. ) ;
#3820 = FACE_OUTER_BOUND ( 'NONE', #18493, .T. ) ;
#3821 = DIRECTION ( 'NONE',  ( 7.087422195345011518E-32, 1.000000000000000000, -0.000000000000000000 ) ) ;
#3822 = CARTESIAN_POINT ( 'NONE',  ( -1.656854249492380582, 4.000000000000000000, -2.887499999999997069 ) ) ;
#3823 = ORIENTED_EDGE ( 'NONE', *, *, #19180, .T. ) ;
#3824 = DIRECTION ( 'NONE',  ( -0.000000000000000000, -0.000000000000000000, -1.000000000000000000 ) ) ;
#3825 = VERTEX_POINT ( 'NONE', #20805 ) ;
#3826 = CARTESIAN_POINT ( 'NONE',  ( 2.828427124746190735, -2.828427124746189847, 1.675000000000001155 ) ) ;
#3827 = EDGE_CURVE ( 'NONE', #6742, #10547, #2837, .T. ) ;
#3828 = CARTESIAN_POINT ( 'NONE',  ( 1.971781867644420635E-15, -4.000000000000000000, 16.25000000000001066 ) ) ;
#3829 = CARTESIAN_POINT ( 'NONE',  ( -2.000000000000001776, 0.000000000000000000, 0.000000000000000000 ) ) ;
#3830 = AXIS2_PLACEMENT_3D ( 'NONE', #443, #7768, #3798 ) ;
#3831 = DIRECTION ( 'NONE',  ( -0.000000000000000000, -1.000000000000000000, -0.000000000000000000 ) ) ;
#3832 = EDGE_CURVE ( 'NONE', #6714, #19393, #6216, .T. ) ;
#3833 = ORIENTED_EDGE ( 'NONE', *, *, #20301, .F. ) ;
#3834 = AXIS2_PLACEMENT_3D ( 'NONE', #11641, #2137, #13307 ) ;
#3835 = EDGE_CURVE ( 'NONE', #21424, #20390, #19139, .T. ) ;
#3836 = VECTOR ( 'NONE', #1682, 1000.000000000000000 ) ;
#3837 = CARTESIAN_POINT ( 'NONE',  ( -11.83859044676619199, -9.000000000000003553, 5.000000000000079936 ) ) ;
#3838 = VECTOR ( 'NONE', #16086, 1000.000000000000000 ) ;
#3839 = DIRECTION ( 'NONE',  ( -1.000000000000000000, 0.000000000000000000, 1.224646799147353207E-16 ) ) ;
#3840 = CARTESIAN_POINT ( 'NONE',  ( 68.00000000109247367, 10.85617417291294551, 17.06698729999999742 ) ) ;
#3841 = CARTESIAN_POINT ( 'NONE',  ( 1.432654583217643163, -3.458734124999999437, 17.75000000136560629 ) ) ;
#3842 = FACE_OUTER_BOUND ( 'NONE', #12830, .T. ) ;
#3843 = CARTESIAN_POINT ( 'NONE',  ( 6.353591512924457348E-16, -3.458734125000000770, -2.762499998634404097 ) ) ;
#3844 = B_SPLINE_CURVE_WITH_KNOTS ( 'NONE', 3,
 ( #12953, #20095, #1903, #9245, #222 ),
 .UNSPECIFIED., .F., .F.,
 ( 4, 1, 4 ),
 ( 0.000000000000000000, 0.002309401076758505790, 0.004618802153517011580 ),
 .UNSPECIFIED. ) ;
#3845 = DIRECTION ( 'NONE',  ( 0.3420201433256622736, -0.9396926207859106484, -1.232595164407828100E-31 ) ) ;
#3846 = CARTESIAN_POINT ( 'NONE',  ( 1.872352939448454495E-15, -3.458734125000000326, 11.68750000136560629 ) ) ;
#3847 = CARTESIAN_POINT ( 'NONE',  ( -1.800000000000000711, 1.077689183249673564E-15, 8.800000000000022027 ) ) ;
#3848 = VERTEX_POINT ( 'NONE', #13652 ) ;
#3849 = CARTESIAN_POINT ( 'NONE',  ( -70.60000000109246798, 7.933012699999995476, 15.85617417291294196 ) ) ;
#3850 = VERTEX_POINT ( 'NONE', #10066 ) ;
#3851 = CARTESIAN_POINT ( 'NONE',  ( 55.27893183416158251, 8.411196891453236901, 10.97181229448535511 ) ) ;
#3852 = CARTESIAN_POINT ( 'NONE',  ( -69.75000000109245946, 11.46158073645647235, 16.46158073645647235 ) ) ;
#3853 = ITEM_DEFINED_TRANSFORMATION ( 'NONE', 'NONE', #14150,  #7318 ) ;
#3854 = LINE ( 'NONE', #9382, #963 ) ;
#3855 = ORIENTED_EDGE ( 'NONE', *, *, #14702, .F. ) ;
#3856 = CIRCLE ( 'NONE', #11923, 6.500000000000000888 ) ;
#3857 = ORIENTED_EDGE ( 'NONE', *, *, #1176, .T. ) ;
#3858 = CARTESIAN_POINT ( 'NONE',  ( 71.09999999999999432, 7.499999999999996447, 14.99999999999999645 ) ) ;
#3859 = CARTESIAN_POINT ( 'NONE',  ( 57.56250000000000000, 6.999999999999997335, 15.00000000000000533 ) ) ;
#3860 = CARTESIAN_POINT ( 'NONE',  ( -70.90000000109246514, 10.85617417291294551, 12.93301269999999370 ) ) ;
#3861 = EDGE_CURVE ( 'NONE', #22477, #11666, #2883, .T. ) ;
#3862 = CARTESIAN_POINT ( 'NONE',  ( -71.40000000109246514, 10.85617417291294551, 17.06698729999999742 ) ) ;
#3863 = CARTESIAN_POINT ( 'NONE',  ( 1.025207404391860050E-15, 3.458734125000000770, 12.43750000136560629 ) ) ;
#3864 = DIRECTION ( 'NONE',  ( 1.000000000000000000, 0.000000000000000000, 0.000000000000000000 ) ) ;
#3865 = CARTESIAN_POINT ( 'NONE',  ( 54.93750000000000711, 10.00000000000000711, 17.99999999999999645 ) ) ;
#3866 = AXIS2_PLACEMENT_3D ( 'NONE', #20679, #8847, #10175 ) ;
#3867 = PLANE ( 'NONE',  #18289 ) ;
#3868 = CARTESIAN_POINT ( 'NONE',  ( 51.28125000000000000, 8.757359312880703683, 11.99999999999999822 ) ) ;
#3869 = CARTESIAN_POINT ( 'NONE',  ( 2.828427124746191179, 2.828427124746190291, 14.75000000273119660 ) ) ;
#3870 = CARTESIAN_POINT ( 'NONE',  ( 1.799999999999996048, 7.347880794884147346E-16, 6.000000000000023093 ) ) ;
#3871 = VERTEX_POINT ( 'NONE', #15580 ) ;
#3872 = DIRECTION ( 'NONE',  ( 1.000000000000000000, 0.000000000000000000, 0.000000000000000000 ) ) ;
#3873 = CARTESIAN_POINT ( 'NONE',  ( -71.60000000218494165, 12.50000000000000000, 14.99999999999999645 ) ) ;
#3874 = EDGE_LOOP ( 'NONE', ( #14418, #21594 ) ) ;
#3875 = CARTESIAN_POINT ( 'NONE',  ( 52.96875000000000000, 6.999999999999992895, 13.75735931288071967 ) ) ;
#3876 = SURFACE_STYLE_USAGE ( .BOTH. , #13007 ) ;
#3877 = CARTESIAN_POINT ( 'NONE',  ( 3.458734125000000326, 4.235727675282971730E-16, 4.237500001365595459 ) ) ;
#3878 = DIRECTION ( 'NONE',  ( -0.000000000000000000, -0.000000000000000000, 1.000000000000000000 ) ) ;
#3879 = ORIENTED_EDGE ( 'NONE', *, *, #14404, .F. ) ;
#3880 = CARTESIAN_POINT ( 'NONE',  ( 2.828427124746191179, 2.828427124746190291, 15.62500000000001066 ) ) ;
#3881 = CARTESIAN_POINT ( 'NONE',  ( 7.347880794884118750E-16, -4.000000000000000000, -2.449999999999998845 ) ) ;
#3882 = FACE_OUTER_BOUND ( 'NONE', #22931, .T. ) ;
#3883 = ORIENTED_EDGE ( 'NONE', *, *, #14071, .F. ) ;
#3884 = LINE ( 'NONE', #16592, #12923 ) ;
#3885 = CARTESIAN_POINT ( 'NONE',  ( 3.458734125000000770, 4.235727675282972223E-16, 0.4875000013655969577 ) ) ;
#3886 = CARTESIAN_POINT ( 'NONE',  ( 68.95000000000000284, 11.03553390593273598, 12.49999999999999289 ) ) ;
#3887 = CARTESIAN_POINT ( 'NONE',  ( 50.00000000000000000, 2.399706452296377357, 55.00000000000021316 ) ) ;
#3888 = CARTESIAN_POINT ( 'NONE',  ( -66.99999999999998579, 8.232233047033627571, 16.76776695296636532 ) ) ;
#3889 = CARTESIAN_POINT ( 'NONE',  ( 50.28356816583843880, 8.275094609561968184, 11.02818770551464667 ) ) ;
#3890 = CARTESIAN_POINT ( 'NONE',  ( -2.445694354108820523, 2.445694354108820523, -0.3874999986344038194 ) ) ;
#3891 = CARTESIAN_POINT ( 'NONE',  ( 3.458734125000002546, -1.432654583217639610, 16.12500000136560629 ) ) ;
#3892 = CARTESIAN_POINT ( 'NONE',  ( 35.27605445928345063, -8.974600000000002353, 5.000000000000079936 ) ) ;
#3893 = CARTESIAN_POINT ( 'NONE',  ( -71.45000000109247651, 9.999999999999998224, 17.06698730000000097 ) ) ;
#3894 = EDGE_CURVE ( 'NONE', #7429, #13541, #9042, .T. ) ;
#3895 = CARTESIAN_POINT ( 'NONE',  ( 71.29999999999998295, 9.999999999999998224, 12.49999999999999289 ) ) ;
#3896 = ORIENTED_EDGE ( 'NONE', *, *, #4429, .T. ) ;
#3897 = CARTESIAN_POINT ( 'NONE',  ( 45.00000000000000000, 15.00000000000003375, 34.11836509645780069 ) ) ;
#3898 =( BOUNDED_CURVE ( )  B_SPLINE_CURVE ( 2, ( #6743, #21682, #1212, #12512, #1570, #10832, #21202, #17993, #19772, #6856, #5293, #15856, #14181, #5054, #10716, #14419, #4816, #1447, #8784, #16203, #7102, #1095, #16089, #8441, #23376, #12148, #6979, #21558, #130, #3849, #1686, #23614, #18221, #18345, #11184, #5644, #7577, #7228, #21914, #12978, #16668, #14896, #16790, #22153, #3603, #13211, #10942, #1804, #242, #9491, #14544, #11059, #9030, #18458, #15020, #4082, #12749, #9151, #19, #22274, #5887, #5412, #16437, #20001, #18106, #3717, #5772, #7352, #20480, #14657, #13099, #12858, #2154, #18573, #5524, #21810, #20242, #16323, #3963, #370, #2039, #20114, #16554, #20355, #11299, #9377, #7703, #1925, #9267, #7459, #14775, #22027, #4206, #8058, #15372, #8172, #6244, #15605, #20598, #838, #10093, #6126, #13330, #11547, #13455, #18695, #2285, #603, #17271, #4562, #9849, #11662, #18816, #22640, #13564, #9980, #11898, #9623, #15485, #22395, #9733, #20833, #20717, #16914, #17147, #2636, #4441, #13681, #18930 ),
 .UNSPECIFIED., .F., .F. ) 
 B_SPLINE_CURVE_WITH_KNOTS ( ( 3, 2, 2, 2, 2, 2, 2, 2, 2, 2, 2, 2, 2, 2, 2, 2, 2, 2, 2, 2, 2, 2, 2, 2, 2, 2, 2, 2, 2, 2, 2, 2, 2, 2, 2, 2, 2, 2, 2, 2, 2, 2, 2, 2, 2, 2, 2, 2, 2, 2, 2, 2, 2, 2, 2, 2, 2, 2, 2, 2, 2, 2, 2, 2, 3 ),
 ( 0.000000000000000000, 0.01562500000000000000, 0.03125000000000000000, 0.04687500000000000000, 0.06250000000000000000, 0.07812500000000000000, 0.09375000000000000000, 0.1093750000000000000, 0.1250000000000000000, 0.1406250000000000000, 0.1562500000000000000, 0.1718750000000000000, 0.1875000000000000000, 0.2031250000000000000, 0.2187500000000000000, 0.2343750000000000000, 0.2500000000000000000, 0.2656250000000000000, 0.2812500000000000000, 0.2968750000000000000, 0.3125000000000000000, 0.3281250000000000000, 0.3437500000000000000, 0.3593750000000000000, 0.3750000000000000000, 0.3906250000000000000, 0.4062500000000000000, 0.4218750000000000000, 0.4375000000000000000, 0.4531250000000000000, 0.4687500000000000000, 0.4843750000000000000, 0.5000000000000000000, 0.5156250000000000000, 0.5312500000000000000, 0.5468750000000000000, 0.5625000000000000000, 0.5781250000000000000, 0.5937500000000000000, 0.6093750000000000000, 0.6250000000000000000, 0.6406250000000000000, 0.6562500000000000000, 0.6718750000000000000, 0.6875000000000000000, 0.7031250000000000000, 0.7187500000000000000, 0.7343750000000000000, 0.7500000000000000000, 0.7656250000000000000, 0.7812500000000000000, 0.7968750000000000000, 0.8125000000000000000, 0.8281250000000000000, 0.8437500000000000000, 0.8593750000000000000, 0.8750000000000000000, 0.8906250000000000000, 0.9062500000000000000, 0.9218750000000000000, 0.9375000000000000000, 0.9531250000000000000, 0.9687500000000000000, 0.9843750000000000000, 1.000000000000000000 ),
 .UNSPECIFIED. ) 
 CURVE ( )  GEOMETRIC_REPRESENTATION_ITEM ( )  RATIONAL_B_SPLINE_CURVE ( ( 1.000000000000000000, 0.9238795325112867385, 1.000000000000000000, 0.9238795325112867385, 1.000000000000000000, 0.9238795325112867385, 1.000000000000000000, 0.9238795325112867385, 1.000000000000000000, 0.9238795325112867385, 1.000000000000000000, 0.9238795325112867385, 1.000000000000000000, 0.9238795325112867385, 1.000000000000000000, 0.9238795325112867385, 1.000000000000000000, 0.9238795325112867385, 1.000000000000000000, 0.9238795325112867385, 1.000000000000000000, 0.9238795325112867385, 1.000000000000000000, 0.9238795325112867385, 1.000000000000000000, 0.9238795325112867385, 1.000000000000000000, 0.9238795325112867385, 1.000000000000000000, 0.9238795325112867385, 1.000000000000000000, 0.9238795325112867385, 1.000000000000000000, 0.9238795325112867385, 1.000000000000000000, 0.9238795325112867385, 1.000000000000000000, 0.9238795325112867385, 1.000000000000000000, 0.9238795325112867385, 1.000000000000000000, 0.9238795325112867385, 1.000000000000000000, 0.9238795325112867385, 1.000000000000000000, 0.9238795325112867385, 1.000000000000000000, 0.9238795325112867385, 1.000000000000000000, 0.9238795325112867385, 1.000000000000000000, 0.9238795325112867385, 1.000000000000000000, 0.9238795325112867385, 1.000000000000000000, 0.9238795325112867385, 1.000000000000000000, 0.9238795325112867385, 1.000000000000000000, 0.9238795325112867385, 1.000000000000000000, 0.9238795325112867385, 1.000000000000000000, 0.9238795325112867385, 1.000000000000000000, 0.9238795325112867385, 1.000000000000000000, 0.9238795325112867385, 1.000000000000000000, 0.9238795325112867385, 1.000000000000000000, 0.9238795325112867385, 1.000000000000000000, 0.9238795325112867385, 1.000000000000000000, 0.9238795325112867385, 1.000000000000000000, 0.9238795325112867385, 1.000000000000000000, 0.9238795325112867385, 1.000000000000000000, 0.9238795325112867385, 1.000000000000000000, 0.9238795325112867385, 1.000000000000000000, 0.9238795325112867385, 1.000000000000000000, 0.9238795325112867385, 1.000000000000000000, 0.9238795325112867385, 1.000000000000000000, 0.9238795325112867385, 1.000000000000000000, 0.9238795325112867385, 1.000000000000000000, 0.9238795325112867385, 1.000000000000000000, 0.9238795325112867385, 1.000000000000000000, 0.9238795325112867385, 1.000000000000000000, 0.9238795325112867385, 1.000000000000000000, 0.9238795325112867385, 1.000000000000000000, 0.9238795325112867385, 1.000000000000000000, 0.9238795325112867385, 1.000000000000000000, 0.9238795325112867385, 1.000000000000000000, 0.9238795325112867385, 1.000000000000000000, 0.9238795325112867385, 1.000000000000000000, 0.9238795325112867385, 1.000000000000000000, 0.9238795325112867385, 1.000000000000000000, 0.9238795325112867385, 1.000000000000000000, 0.9238795325112867385, 1.000000000000000000, 0.9238795325112867385, 1.000000000000000000, 0.9238795325112867385, 1.000000000000000000, 0.9238795325112867385, 1.000000000000000000 ) ) 
 REPRESENTATION_ITEM ( '' )  );
#3899 = CARTESIAN_POINT ( 'NONE',  ( 24.42673246966726452, -11.25000000000000355, 10.00000000000008882 ) ) ;
#3900 = FACE_OUTER_BOUND ( 'NONE', #3340, .T. ) ;
#3901 = ORIENTED_EDGE ( 'NONE', *, *, #16314, .T. ) ;
#3902 = VERTEX_POINT ( 'NONE', #13891 ) ;
#3903 = EDGE_CURVE ( 'NONE', #14683, #18117, #17096, .T. ) ;
#3904 = CARTESIAN_POINT ( 'NONE',  ( 55.50000000000000711, 12.82842712474617741, 12.17157287525379239 ) ) ;
#3905 = VERTEX_POINT ( 'NONE', #16033 ) ;
#3906 = ORIENTED_EDGE ( 'NONE', *, *, #15603, .T. ) ;
#3907 = CARTESIAN_POINT ( 'NONE',  ( 52.34606816583843880, 8.411196891453267099, 19.02818770551464667 ) ) ;
#3908 = VECTOR ( 'NONE', #23073, 1000.000000000000000 ) ;
#3909 = CARTESIAN_POINT ( 'NONE',  ( 66.10000000218495586, 11.76776695296636888, 16.76776695296636532 ) ) ;
#3910 = DIRECTION ( 'NONE',  ( 0.000000000000000000, 0.000000000000000000, 1.000000000000000000 ) ) ;
#3911 = CARTESIAN_POINT ( 'NONE',  ( 71.75000000109247367, 8.538419263543524096, 13.53841926354352054 ) ) ;
#3912 = VERTEX_POINT ( 'NONE', #23322 ) ;
#3913 = CARTESIAN_POINT ( 'NONE',  ( -2.828427124746189403, 2.828427124746190291, 19.00000000273119838 ) ) ;
#3914 = DIRECTION ( 'NONE',  ( 0.000000000000000000, 0.000000000000000000, -1.000000000000000000 ) ) ;
#3915 = CARTESIAN_POINT ( 'NONE',  ( 56.77893183416158251, 8.411196891453236901, 10.97181229448535511 ) ) ;
#3916 = DIRECTION ( 'NONE',  ( 1.000000000000000000, 0.000000000000000000, 0.000000000000000000 ) ) ;
#3917 = CARTESIAN_POINT ( 'NONE',  ( 6.499999999999999112, 0.000000000000000000, 2.040000000000001812 ) ) ;
#3918 = CARTESIAN_POINT ( 'NONE',  ( 14.99999999999996092, -15.00000000000000000, -20.00000000000000355 ) ) ;
#3919 = ADVANCED_FACE ( 'NONE', ( #2954 ), #1271, .T. ) ;
#3920 = CARTESIAN_POINT ( 'NONE',  ( -19.99999999999999645, -9.000000000000003553, 5.000000000000079936 ) ) ;
#3921 = FACE_OUTER_BOUND ( 'NONE', #7813, .T. ) ;
#3922 = EDGE_LOOP ( 'NONE', ( #18403, #14686, #11774, #18278 ) ) ;
#3923 = CARTESIAN_POINT ( 'NONE',  ( 44.00000000000000711, -9.000000000000003553, 11.00000000000008882 ) ) ;
#3924 = EDGE_CURVE ( 'NONE', #7419, #15377, #22135, .T. ) ;
#3925 = CARTESIAN_POINT ( 'NONE',  ( -4.203934362469166963, -1.640673743454851286, -3.598432614606932756 ) ) ;
#3926 = CYLINDRICAL_SURFACE ( 'NONE', #3950, 2.100000000000000089 ) ;
#3927 = AXIS2_PLACEMENT_3D ( 'NONE', #13450, #22511, #22024 ) ;
#3928 = ORIENTED_EDGE ( 'NONE', *, *, #6138, .T. ) ;
#3929 = CARTESIAN_POINT ( 'NONE',  ( 4.000000000000000888, 4.898587196589412829E-16, 13.50000000000001066 ) ) ;
#3930 = CARTESIAN_POINT ( 'NONE',  ( 70.70000000000000284, 12.50000000000000000, 14.99999999999999645 ) ) ;
#3931 = CARTESIAN_POINT ( 'NONE',  ( -6.500000000000000000, 3.752776749732564809, -0.5805565836007661185 ) ) ;
#3932 = CIRCLE ( 'NONE', #4712, 4.000000000000001776 ) ;
#3933 = EDGE_CURVE ( 'NONE', #6742, #12252, #14248, .T. ) ;
#3934 = CARTESIAN_POINT ( 'NONE',  ( 4.000000000000001776, -1.656854249492379694, 16.56250000273119838 ) ) ;
#3935 = ORIENTED_EDGE ( 'NONE', *, *, #10441, .F. ) ;
#3936 = CARTESIAN_POINT ( 'NONE',  ( 4.000000000000000000, 2.309401076758515803, -0.4999999999999995559 ) ) ;
#3937 = ORIENTED_EDGE ( 'NONE', *, *, #16094, .F. ) ;
#3938 = EDGE_CURVE ( 'NONE', #6517, #11847, #5709, .T. ) ;
#3939 =( BOUNDED_CURVE ( )  B_SPLINE_CURVE ( 2, ( #5287, #14653, #12631, #10712, #20110, #16319, #17867, #23609, #11054 ),
 .UNSPECIFIED., .F., .F. ) 
 B_SPLINE_CURVE_WITH_KNOTS ( ( 3, 2, 2, 2, 3 ),
 ( 0.4999999999999991118, 0.5156249999999995559, 0.5312500000000000000, 0.5468750000000004441, 0.5625000000000008882 ),
 .UNSPECIFIED. ) 
 CURVE ( )  GEOMETRIC_REPRESENTATION_ITEM ( )  RATIONAL_B_SPLINE_CURVE ( ( 1.000000000000004219, 0.9238795325112824086, 1.000000000000000000, 0.9238795325112867385, 1.000000000000000000, 0.9238795325112867385, 1.000000000000000000, 0.9238795325112824086, 1.000000000000004219 ) ) 
 REPRESENTATION_ITEM ( '' )  );
#3940 = CARTESIAN_POINT ( 'NONE',  ( -2.828427124746189403, -2.828427124746190735, 1.425000000000000933 ) ) ;
#3941 = CARTESIAN_POINT ( 'NONE',  ( 4.000000000000001776, -1.656854249492379694, 14.43750000000001066 ) ) ;
#3942 = CARTESIAN_POINT ( 'NONE',  ( -5.432802636760778014, 4.368923434677190798, -3.442664554191217530 ) ) ;
#3943 = APPLICATION_CONTEXT ( 'automotive_design' ) ;
#3944 = CARTESIAN_POINT ( 'NONE',  ( 60.00000000000000000, -10.00000000000000178, 14.99999999999999467 ) ) ;
#3945 = PRESENTATION_STYLE_ASSIGNMENT (( #22624 ) ) ;
#3946 = CARTESIAN_POINT ( 'NONE',  ( 70.35000000109246798, 11.46158073645647235, 13.53841926354352232 ) ) ;
#3947 = EDGE_LOOP ( 'NONE', ( #16861, #17027, #19713 ) ) ;
#3948 = AXIS2_PLACEMENT_3D ( 'NONE', #10802, #7430, #7193 ) ;
#3949 = CARTESIAN_POINT ( 'NONE',  ( 45.00000000000000000, -15.00000000000001954, 10.00000000000008882 ) ) ;
#3950 = AXIS2_PLACEMENT_3D ( 'NONE', #9346, #7322, #14862 ) ;
#3951 = ADVANCED_FACE ( 'NONE', ( #8608 ), #8099, .T. ) ;
#3952 = CARTESIAN_POINT ( 'NONE',  ( 66.25000000218494733, 8.964466094067207180, 17.49999999999995026 ) ) ;
#3953 = CARTESIAN_POINT ( 'NONE',  ( 67.15000000109247935, 11.46158073645647235, 16.46158073645647235 ) ) ;
#3954 = CARTESIAN_POINT ( 'NONE',  ( 1.432654583217641164, 3.458734125000000326, 17.12500000136560629 ) ) ;
#3955 = PLANE ( 'NONE',  #19685 ) ;
#3956 = CARTESIAN_POINT ( 'NONE',  ( -1.432654583217641164, -3.458734125000000326, -2.824999998634404985 ) ) ;
#3957 = CARTESIAN_POINT ( 'NONE',  ( -2.828427124746190291, 2.828427124746190291, 4.174999999999999822 ) ) ;
#3958 = ADVANCED_FACE ( 'NONE', ( #21523 ), #14383, .F. ) ;
#3959 = DIRECTION ( 'NONE',  ( -7.087422195345011518E-32, -1.000000000000000000, -0.000000000000000000 ) ) ;
#3960 = CARTESIAN_POINT ( 'NONE',  ( 3.458734125000001214, 1.432654583217640498, 14.00000000136560629 ) ) ;
#3961 = CYLINDRICAL_SURFACE ( 'NONE', #17621, 4.000000000000000000 ) ;
#3962 = ORIENTED_EDGE ( 'NONE', *, *, #23567, .T. ) ;
#3963 = CARTESIAN_POINT ( 'NONE',  ( -68.15000000109247935, 8.538419263543522320, 16.46158073645647235 ) ) ;
#3964 = ORIENTED_EDGE ( 'NONE', *, *, #21194, .F. ) ;
#3965 = CARTESIAN_POINT ( 'NONE',  ( 59.25000000000000711, 7.171572875253819923, 17.82842712474619873 ) ) ;
#3966 = CARTESIAN_POINT ( 'NONE',  ( -70.15000000109246514, 8.538419263543524096, 13.53841926354352054 ) ) ;
#3967 = SHAPE_DEFINITION_REPRESENTATION ( #22514, #10226 ) ;
#3968 = EDGE_CURVE ( 'NONE', #10612, #19485, #23339, .T. ) ;
#3969 = ORIENTED_EDGE ( 'NONE', *, *, #14033, .T. ) ;
#3970 = CYLINDRICAL_SURFACE ( 'NONE', #2104, 9.000000000000021316 ) ;
#3971 = EDGE_LOOP ( 'NONE', ( #21691, #4448, #8481, #17129 ) ) ;
#3972 = EDGE_CURVE ( 'NONE', #1974, #11365, #19091, .T. ) ;
#3973 = ORIENTED_EDGE ( 'NONE', *, *, #10277, .T. ) ;
#3974 = CARTESIAN_POINT ( 'NONE',  ( 1.432654583217643163, -3.458734124999999882, 17.00000000136560629 ) ) ;
#3975 = CARTESIAN_POINT ( 'NONE',  ( 58.40625000000000711, 12.99999999999999645, 13.75735931288070191 ) ) ;
#3976 = CARTESIAN_POINT ( 'NONE',  ( -67.55000000109247082, 8.538419263543524096, 13.53841926354352054 ) ) ;
#3977 = CARTESIAN_POINT ( 'NONE',  ( 69.15000000109247935, 8.538419263543524096, 13.53841926354352054 ) ) ;
#3978 = CARTESIAN_POINT ( 'NONE',  ( -68.65000000109246514, 9.999999999999998224, 12.93301269999999192 ) ) ;
#3979 = CARTESIAN_POINT ( 'NONE',  ( -3.458734124999998105, -1.432654583217642497, 12.75000000136560629 ) ) ;
#3980 = CARTESIAN_POINT ( 'NONE',  ( -5.007715329123867711E-16, -7.505553499465146494, -3.700000000000000178 ) ) ;
#3981 = CARTESIAN_POINT ( 'NONE',  ( 54.46875000000000000, 6.999999999999992895, 13.75735931288071967 ) ) ;
#3982 = CARTESIAN_POINT ( 'NONE',  ( 0.000000000000000000, 6.772677083992466152, -5.538577986808826736 ) ) ;
#3983 = CARTESIAN_POINT ( 'NONE',  ( -1.432654583217640498, 3.458734125000000770, 5.800000001365597235 ) ) ;
#3984 = CARTESIAN_POINT ( 'NONE',  ( -1.432654583217639610, -3.458734124999999882, 11.62500000136560629 ) ) ;
#3985 = CARTESIAN_POINT ( 'NONE',  ( 1.656854249492384135, -3.999999999999999112, 15.43750000273119660 ) ) ;
#3986 = VECTOR ( 'NONE', #15626, 1000.000000000000000 ) ;
#3987 = CARTESIAN_POINT ( 'NONE',  ( 68.49999999999998579, 9.999999999999998224, 17.49999999999999645 ) ) ;
#3988 = VERTEX_POINT ( 'NONE', #15820 ) ;
#3989 = CARTESIAN_POINT ( 'NONE',  ( 11.86036186966726191, -11.25000000000000355, 5.000000000000079936 ) ) ;
#3990 = CARTESIAN_POINT ( 'NONE',  ( 1.236993788156008760E-15, 0.000000000000000000, 21.31370849898476649 ) ) ;
#3991 = ORIENTED_EDGE ( 'NONE', *, *, #9236, .T. ) ;
#3992 = CARTESIAN_POINT ( 'NONE',  ( 58.09143183416158962, 11.31069182806491291, 12.02818770551463778 ) ) ;
#3993 = CARTESIAN_POINT ( 'NONE',  ( 6.353591512924457348E-16, -3.458734125000000326, 4.987500001365595459 ) ) ;
#3994 = VECTOR ( 'NONE', #13641, 1000.000000000000000 ) ;
#3995 = ADVANCED_FACE ( 'NONE', ( #19504 ), #6818, .T. ) ;
#3996 = CARTESIAN_POINT ( 'NONE',  ( 50.00000000000000000, 7.098169556225943033, 56.71010071662853136 ) ) ;
#3997 = ORIENTED_EDGE ( 'NONE', *, *, #11431, .T. ) ;
#3998 = CARTESIAN_POINT ( 'NONE',  ( -1.656854249492380138, -3.999999999999999112, 12.18750000000001066 ) ) ;
#3999 = ADVANCED_FACE ( 'NONE', ( #11019 ), #16516, .T. ) ;
#4000 = DIRECTION ( 'NONE',  ( -1.000000000000000000, -0.000000000000000000, -0.000000000000000000 ) ) ;
#4001 = CIRCLE ( 'NONE', #5146, 2.649999999999999467 ) ;
#4002 = VECTOR ( 'NONE', #12473, 1000.000000000000000 ) ;
#4003 = DIRECTION ( 'NONE',  ( 0.3420201433256622736, 0.9396926207859106484, 0.000000000000000000 ) ) ;
#4004 = VERTEX_POINT ( 'NONE', #16628 ) ;
#4005 = CARTESIAN_POINT ( 'NONE',  ( 72.50000000000000000, 9.999999999999998224, 14.99999999999999645 ) ) ;
#4006 = CARTESIAN_POINT ( 'NONE',  ( 0.000000000000000000, 0.000000000000000000, 0.000000000000000000 ) ) ;
#4007 = CARTESIAN_POINT ( 'NONE',  ( 68.39999999999999147, 11.76776695296636888, 16.76776695296636532 ) ) ;
#4008 = CARTESIAN_POINT ( 'NONE',  ( -4.000000000000000000, 4.898587196589412829E-16, 19.04999999999996874 ) ) ;
#4009 = AXIS2_PLACEMENT_3D ( 'NONE', #9123, #7677, #15105 ) ;
#4010 = CARTESIAN_POINT ( 'NONE',  ( -90.00000000000000000, 9.887492094615969966E-16, 8.073750000000021743 ) ) ;
#4011 = CARTESIAN_POINT ( 'NONE',  ( 58.43981816583843170, 10.06805114094563791, 17.99999999999999645 ) ) ;
#4012 = VECTOR ( 'NONE', #21254, 1000.000000000000000 ) ;
#4013 = CARTESIAN_POINT ( 'NONE',  ( 1.432654583217639832, 3.458734125000000326, -2.574999998634404541 ) ) ;
#4014 = CARTESIAN_POINT ( 'NONE',  ( 3.458734125000001658, 4.235727675282972223E-16, 13.18750000136560452 ) ) ;
#4015 = CARTESIAN_POINT ( 'NONE',  ( -72.09999999999999432, 9.999999999999998224, 12.49999999999999289 ) ) ;
#4016 = CARTESIAN_POINT ( 'NONE',  ( 54.99999999999996447, 15.00000000000000000, 5.000000000000003553 ) ) ;
#4017 = B_SPLINE_CURVE_WITH_KNOTS ( 'NONE', 3,
 ( #1798, #3492, #5166, #18217, #10938, #14176 ),
 .UNSPECIFIED., .F., .F.,
 ( 4, 2, 4 ),
 ( 0.000000000000000000, 0.5000000000000000000, 1.000000000000000000 ),
 .UNSPECIFIED. ) ;
#4018 = DIRECTION ( 'NONE',  ( 0.000000000000000000, 0.000000000000000000, 1.000000000000000000 ) ) ;
#4019 = VERTEX_POINT ( 'NONE', #7537 ) ;
#4020 = CARTESIAN_POINT ( 'NONE',  ( 3.254516946766202512, -9.000000000000001776, 5.000000000000079936 ) ) ;
#4021 = CARTESIAN_POINT ( 'NONE',  ( -19.99999999999999645, -9.000000000000003553, 5.000000000000079936 ) ) ;
#4022 = CARTESIAN_POINT ( 'NONE',  ( -69.05000000109247082, 7.933012699999995476, 14.99999999999999645 ) ) ;
#4023 = ORIENTED_EDGE ( 'NONE', *, *, #8948, .F. ) ;
#4024 = ORIENTED_EDGE ( 'NONE', *, *, #2061, .F. ) ;
#4025 = CARTESIAN_POINT ( 'NONE',  ( 0.000000000000000000, 6.807171995660675101, -6.478011392632816445 ) ) ;
#4026 = B_SPLINE_CURVE_WITH_KNOTS ( 'NONE', 3,
 ( #12248, #19516, #17734, #15937, #2127, #18198 ),
 .UNSPECIFIED., .F., .F.,
 ( 4, 2, 4 ),
 ( 2.380733003149298079E-07, 0.001898835937927375499, 0.003797433802554436334 ),
 .UNSPECIFIED. ) ;
#4027 = CARTESIAN_POINT ( 'NONE',  ( 58.31250000000000000, 14.00000000000000000, 14.99999999999997691 ) ) ;
#4028 = ORIENTED_EDGE ( 'NONE', *, *, #9524, .F. ) ;
#4029 = EDGE_LOOP ( 'NONE', ( #10625, #13086, #18682, #9526 ) ) ;
#4030 = UNCERTAINTY_MEASURE_WITH_UNIT (LENGTH_MEASURE( 1.000000000000000082E-05 ), #9057, 'distance_accuracy_value', 'NONE');
#4031 = CARTESIAN_POINT ( 'NONE',  ( 54.03356816583844591, 11.72490539043803004, 18.97181229448534268 ) ) ;
#4032 = CIRCLE ( 'NONE', #21996, 8.749000000000000554 ) ;
#4033 = CARTESIAN_POINT ( 'NONE',  ( 65.45000000218496439, 8.964466094067258695, 17.50000000000000355 ) ) ;
#4034 = EDGE_CURVE ( 'NONE', #19393, #4326, #5843, .T. ) ;
#4035 = CARTESIAN_POINT ( 'NONE',  ( -2.828427124746189403, 2.828427124746190291, 19.87500000000001066 ) ) ;
#4036 = CARTESIAN_POINT ( 'NONE',  ( 71.90000000109246514, 10.85617417291294551, 12.93301269999999370 ) ) ;
#4037 = VERTEX_POINT ( 'NONE', #9582 ) ;
#4038 = CARTESIAN_POINT ( 'NONE',  ( 4.000000000000000888, 4.898587196589412829E-16, 15.62500000273119660 ) ) ;
#4039 = VECTOR ( 'NONE', #6456, 1000.000000000000000 ) ;
#4040 = CIRCLE ( 'NONE', #9416, 4.000000000000000000 ) ;
#4041 = DIRECTION ( 'NONE',  ( 0.000000000000000000, 0.000000000000000000, 1.000000000000000000 ) ) ;
#4042 =( BOUNDED_CURVE ( )  B_SPLINE_CURVE ( 2, ( #14813, #18033, #18379, #10977, #9414, #10758, #14694, #16588, #21952 ),
 .UNSPECIFIED., .F., .F. ) 
 B_SPLINE_CURVE_WITH_KNOTS ( ( 3, 2, 2, 2, 3 ),
 ( 0.4999999999999991118, 0.5156249999999995559, 0.5312500000000000000, 0.5468750000000004441, 0.5625000000000008882 ),
 .UNSPECIFIED. ) 
 CURVE ( )  GEOMETRIC_REPRESENTATION_ITEM ( )  RATIONAL_B_SPLINE_CURVE ( ( 1.000000000000004219, 0.9238795325112824086, 1.000000000000000000, 0.9238795325112867385, 1.000000000000000000, 0.9238795325112867385, 1.000000000000000000, 0.9238795325112824086, 1.000000000000004219 ) ) 
 REPRESENTATION_ITEM ( '' )  );
#4043 = CARTESIAN_POINT ( 'NONE',  ( 52.56018183416157541, 5.999999999999996447, 14.93194885905437808 ) ) ;
#4044 = CARTESIAN_POINT ( 'NONE',  ( 3.602667665204950076, -0.9740173600655226416, 2.039999999999998703 ) ) ;
#4045 = DIRECTION ( 'NONE',  ( -0.000000000000000000, -0.000000000000000000, 1.000000000000000000 ) ) ;
#4046 = LINE ( 'NONE', #20437, #19310 ) ;
#4047 = DIRECTION ( 'NONE',  ( 0.000000000000000000, -0.8090169943749403458, -0.5877852522924830181 ) ) ;
#4048 = AXIS2_PLACEMENT_3D ( 'NONE', #8888, #21660, #15837 ) ;
#4049 = CARTESIAN_POINT ( 'NONE',  ( 65.00000000000000000, -15.00000000000000000, 19.99999999999999645 ) ) ;
#4050 = ORIENTED_EDGE ( 'NONE', *, *, #11223, .T. ) ;
#4051 = CARTESIAN_POINT ( 'NONE',  ( 51.75000000000000711, 7.878679656440361612, 17.12132034355964549 ) ) ;
#4052 = CARTESIAN_POINT ( 'NONE',  ( 15.83013239071656741, -8.974600000000002353, 10.00000000000008882 ) ) ;
#4053 = ORIENTED_EDGE ( 'NONE', *, *, #22032, .F. ) ;
#4054 = DIRECTION ( 'NONE',  ( 0.5000000000000013323, -0.000000000000000000, -0.8660254037844380415 ) ) ;
#4055 = DIRECTION ( 'NONE',  ( -0.000000000000000000, -0.000000000000000000, -1.000000000000000000 ) ) ;
#4056 = CARTESIAN_POINT ( 'NONE',  ( 4.999999999999999112, -9.241976615262146311, 2.300561732649528679 ) ) ;
#4057 = DIRECTION ( 'NONE',  ( -0.000000000000000000, -0.000000000000000000, 1.000000000000000000 ) ) ;
#4058 = ORIENTED_EDGE ( 'NONE', *, *, #22648, .F. ) ;
#4059 = CARTESIAN_POINT ( 'NONE',  ( 45.00000000000000000, 10.00000000000001599, 34.11836509645781490 ) ) ;
#4060 = ORIENTED_EDGE ( 'NONE', *, *, #9816, .F. ) ;
#4061 = CARTESIAN_POINT ( 'NONE',  ( -3.999999999999999112, 1.656854249492380582, 19.06250000273120193 ) ) ;
#4062 = CARTESIAN_POINT ( 'NONE',  ( 4.000000000000000888, 1.656854249492381248, 15.56250000000000888 ) ) ;
#4063 = CARTESIAN_POINT ( 'NONE',  ( -31.74999999999995737, 3.061616997868383634E-16, -2.500000000000000444 ) ) ;
#4064 = ADVANCED_FACE ( 'NONE', ( #3681 ), #20436, .F. ) ;
#4065 = CYLINDRICAL_SURFACE ( 'NONE', #9942, 4.000000000000000000 ) ;
#4066 = EDGE_CURVE ( 'NONE', #2967, #17589, #20221, .T. ) ;
#4067 = CARTESIAN_POINT ( 'NONE',  ( 25.25491034071656316, -8.974600000000002353, 5.000000000000079936 ) ) ;
#4068 = CARTESIAN_POINT ( 'NONE',  ( 70.40000000109247935, 12.06698729999999919, 14.14382582708705094 ) ) ;
#4069 = EDGE_LOOP ( 'NONE', ( #16529, #16721, #18086 ) ) ;
#4070 = CARTESIAN_POINT ( 'NONE',  ( -10.00000000000000000, 0.000000000000000000, 0.000000000000000000 ) ) ;
#4071 = LINE ( 'NONE', #22382, #11470 ) ;
#4072 = EDGE_CURVE ( 'NONE', #15000, #2759, #23296, .T. ) ;
#4073 = CARTESIAN_POINT ( 'NONE',  ( 71.60000000109246798, 7.933012699999995476, 15.85617417291294196 ) ) ;
#4074 = CARTESIAN_POINT ( 'NONE',  ( 3.458734125000001214, 1.432654583217640498, 17.00000000136560629 ) ) ;
#4075 = CARTESIAN_POINT ( 'NONE',  ( -15.58579410928343911, -8.974600000000002353, 5.000000000000079936 ) ) ;
#4076 = CARTESIAN_POINT ( 'NONE',  ( 3.458734125000000770, 4.235727675282972223E-16, -1.512499998634402987 ) ) ;
#4077 = CARTESIAN_POINT ( 'NONE',  ( 1.656854249492383024, -3.999999999999999112, 2.612500000000002043 ) ) ;
#4078 = CARTESIAN_POINT ( 'NONE',  ( -71.05000000218497291, 8.964466094067221391, 17.49999999999996447 ) ) ;
#4079 = CARTESIAN_POINT ( 'NONE',  ( 2.445694354108821855, -2.445694354108820079, 14.81250000136560452 ) ) ;
#4080 = DIRECTION ( 'NONE',  ( 0.000000000000000000, 0.000000000000000000, -1.000000000000000000 ) ) ;
#4081 = VERTEX_POINT ( 'NONE', #3917 ) ;
#4082 = CARTESIAN_POINT ( 'NONE',  ( -69.30000000109247082, 10.85617417291294551, 12.93301269999999192 ) ) ;
#4083 = ORIENTED_EDGE ( 'NONE', *, *, #13845, .F. ) ;
#4084 = CARTESIAN_POINT ( 'NONE',  ( 58.87500000000000711, 7.171572875253794166, 12.17157287525381726 ) ) ;
#4085 = CARTESIAN_POINT ( 'NONE',  ( -65.80000000109247082, 7.933012699999995476, 15.85617417291294196 ) ) ;
#4086 = VERTEX_POINT ( 'NONE', #13061 ) ;
#4087 = CARTESIAN_POINT ( 'NONE',  ( 4.000000000000000000, 1.656854249492381248, 0.9875000027311868767 ) ) ;
#4088 = ORIENTED_EDGE ( 'NONE', *, *, #4824, .F. ) ;
#4089 = ADVANCED_FACE ( 'NONE', ( #13170 ), #453, .T. ) ;
#4090 = ORIENTED_EDGE ( 'NONE', *, *, #22819, .F. ) ;
#4091 = CARTESIAN_POINT ( 'NONE',  ( 3.458734125000001658, 1.432654583217640498, 15.25000000136560807 ) ) ;
#4092 = CARTESIAN_POINT ( 'NONE',  ( 52.96875000000000000, 6.999999999999992895, 13.75735931288071967 ) ) ;
#4093 = AXIS2_PLACEMENT_3D ( 'NONE', #5533, #18005, #19905 ) ;
#4094 = CARTESIAN_POINT ( 'NONE',  ( -67.05000000109247082, 12.06698730000000097, 14.99999999999999645 ) ) ;
#4095 = EDGE_CURVE ( 'NONE', #1550, #1016, #18305, .T. ) ;
#4096 = CARTESIAN_POINT ( 'NONE',  ( 68.35000000109248219, 8.538419263543524096, 13.53841926354352054 ) ) ;
#4097 = AXIS2_PLACEMENT_3D ( 'NONE', #21341, #8813, #10620 ) ;
#4098 = CARTESIAN_POINT ( 'NONE',  ( -66.80000000109247082, 7.933012699999995476, 15.85617417291294196 ) ) ;
#4099 = FACE_OUTER_BOUND ( 'NONE', #369, .T. ) ;
#4100 = ADVANCED_FACE ( 'NONE', ( #21994 ), #22726, .F. ) ;
#4101 = CARTESIAN_POINT ( 'NONE',  ( 55.37268183416157541, 7.926799079670491466, 12.83056023321021755 ) ) ;
#4102 = LINE ( 'NONE', #1945, #21327 ) ;
#4103 = EDGE_CURVE ( 'NONE', #16245, #5234, #5917, .T. ) ;
#4104 = AXIS2_PLACEMENT_3D ( 'NONE', #2018, #18680, #4188 ) ;
#4105 = CARTESIAN_POINT ( 'NONE',  ( -1.432654583217640498, 3.458734125000000770, 3.800000001365595459 ) ) ;
#4106 = CARTESIAN_POINT ( 'NONE',  ( 2.548804901056335857E-15, 4.736522675502163437, -3.681124513963624612 ) ) ;
#4107 = CARTESIAN_POINT ( 'NONE',  ( -1.656854249492379250, 4.000000000000000000, 14.93750000273119660 ) ) ;
#4108 = LINE ( 'NONE', #9286, #21410 ) ;
#4109 = AXIS2_PLACEMENT_3D ( 'NONE', #11749, #2839, #8380 ) ;
#4110 = ORIENTED_EDGE ( 'NONE', *, *, #216, .T. ) ;
#4111 = DIRECTION ( 'NONE',  ( 0.3420201433256622181, -0.9396926207859107594, 0.000000000000000000 ) ) ;
#4112 = ORIENTED_EDGE ( 'NONE', *, *, #13576, .F. ) ;
#4113 = CARTESIAN_POINT ( 'NONE',  ( 55.93518183416157541, 9.931948859054372747, 17.99999999999999645 ) ) ;
#4114 = CARTESIAN_POINT ( 'NONE',  ( -3.458734124999999882, -1.432654583217642497, 3.800000001365595459 ) ) ;
#4115 = CARTESIAN_POINT ( 'NONE',  ( -71.00000000218494733, 9.999999999999998224, 17.49999999999999645 ) ) ;
#4116 = ORIENTED_EDGE ( 'NONE', *, *, #4730, .T. ) ;
#4117 = CARTESIAN_POINT ( 'NONE',  ( 1.656854249492381470, 4.000000000000000000, 14.68750000000000888 ) ) ;
#4118 = CARTESIAN_POINT ( 'NONE',  ( 4.999999999999999112, -9.241976615262169403, 1.699438267350339871 ) ) ;
#4119 = ORIENTED_EDGE ( 'NONE', *, *, #4646, .T. ) ;
#4120 = CIRCLE ( 'NONE', #17887, 5.000000000000011546 ) ;
#4121 = CARTESIAN_POINT ( 'NONE',  ( -71.80000000218494449, 9.999999999999998224, 17.49999999999999645 ) ) ;
#4122 = CARTESIAN_POINT ( 'NONE',  ( 3.458734125000001214, -1.432654583217639610, -0.5749999986344027647 ) ) ;
#4123 = B_SPLINE_CURVE_WITH_KNOTS ( 'NONE', 3,
 ( #4735, #15543, #2920, #11953, #18534, #22808 ),
 .UNSPECIFIED., .F., .F.,
 ( 4, 2, 4 ),
 ( 4.336808689942017736E-19, 0.0002095117440854729585, 0.0004190234881709454834 ),
 .UNSPECIFIED. ) ;
#4124 = VECTOR ( 'NONE', #2433, 1000.000000000000000 ) ;
#4125 = CARTESIAN_POINT ( 'NONE',  ( 4.000000000000000000, 4.898587196589412829E-16, -1.074999997268812679 ) ) ;
#4126 = ADVANCED_FACE ( 'NONE', ( #20316, #11256 ), #11375, .T. ) ;
#4127 = CARTESIAN_POINT ( 'NONE',  ( 66.90000000000000568, 9.999999999999998224, 17.49999999999999645 ) ) ;
#4128 = EDGE_CURVE ( 'NONE', #21720, #18422, #9230, .T. ) ;
#4129 = CARTESIAN_POINT ( 'NONE',  ( -71.00000000000000000, 8.232233047033627571, 16.76776695296636532 ) ) ;
#4130 = EDGE_CURVE ( 'NONE', #3403, #23470, #16747, .T. ) ;
#4131 = CARTESIAN_POINT ( 'NONE',  ( 4.999999999999999112, 0.000000000000000000, 0.000000000000000000 ) ) ;
#4132 = CARTESIAN_POINT ( 'NONE',  ( 55.06481816583844591, 5.999999999999996447, 15.06805114094564502 ) ) ;
#4133 = CARTESIAN_POINT ( 'NONE',  ( -2.445694354108819635, -2.445694354108820523, -3.137499998634404541 ) ) ;
#4134 = CARTESIAN_POINT ( 'NONE',  ( 1.432654583217641386, 3.458734125000000770, 16.37500000136560629 ) ) ;
#4135 = CARTESIAN_POINT ( 'NONE',  ( 68.85000000218495586, 7.499999999999996447, 13.96446609406725514 ) ) ;
#4136 = CARTESIAN_POINT ( 'NONE',  ( 2.499999999999999556, -4.762163868918344534, 9.915734732513202587 ) ) ;
#4137 = AXIS2_PLACEMENT_3D ( 'NONE', #11913, #21187, #15846 ) ;
#4138 = CARTESIAN_POINT ( 'NONE',  ( 25.85127650928345489, -8.974600000000002353, 5.000000000000079936 ) ) ;
#4139 = ORIENTED_EDGE ( 'NONE', *, *, #15537, .F. ) ;
#4140 = CARTESIAN_POINT ( 'NONE',  ( 4.000000000000000000, -1.560351142792952617, -0.2242961665059816367 ) ) ;
#4141 = LINE ( 'NONE', #18507, #16305 ) ;
#4142 = CARTESIAN_POINT ( 'NONE',  ( -71.75000000109248788, 11.46158073645647235, 13.53841926354352232 ) ) ;
#4143 = EDGE_LOOP ( 'NONE', ( #18603, #5082, #17062, #10040 ) ) ;
#4144 = ORIENTED_EDGE ( 'NONE', *, *, #4298, .T. ) ;
#4145 = VECTOR ( 'NONE', #22361, 1000.000000000000000 ) ;
#4146 = PRESENTATION_LAYER_ASSIGNMENT (  '', '', ( #18302 ) ) ;
#4147 = LINE ( 'NONE', #18764, #4505 ) ;
#4148 = VERTEX_POINT ( 'NONE', #22235 ) ;
#4149 = CARTESIAN_POINT ( 'NONE',  ( 50.00000000000000000, -10.00000000000001599, 34.11836509645782201 ) ) ;
#4150 = EDGE_LOOP ( 'NONE', ( #1952, #17659, #7793, #22786 ) ) ;
#4151 = CARTESIAN_POINT ( 'NONE',  ( 52.15856816583843880, 6.028187705514649330, 16.72490539043803182 ) ) ;
#4152 = CARTESIAN_POINT ( 'NONE',  ( 66.05000000218494449, 12.50000000000000000, 16.03553390593273420 ) ) ;
#4153 = AXIS2_PLACEMENT_3D ( 'NONE', #4070, #4426, #20704 ) ;
#4154 = FACE_OUTER_BOUND ( 'NONE', #20298, .T. ) ;
#4155 = EDGE_CURVE ( 'NONE', #6665, #17502, #924, .T. ) ;
#4156 = CARTESIAN_POINT ( 'NONE',  ( 71.70000000109247651, 7.933012699999995476, 14.14382582708705094 ) ) ;
#4157 = ORIENTED_EDGE ( 'NONE', *, *, #8689, .F. ) ;
#4158 = CARTESIAN_POINT ( 'NONE',  ( 9.920644283265380691E-16, 4.000000000000000000, 12.87500000273119660 ) ) ;
#4159 = CARTESIAN_POINT ( 'NONE',  ( -27.50000000000000711, 1.500000000000003109, -31.01025403784446510 ) ) ;
#4160 = CIRCLE ( 'NONE', #16028, 0.5000000000000006661 ) ;
#4161 = CARTESIAN_POINT ( 'NONE',  ( 56.12268183416157541, 12.78030770151606177, 17.87654654797631792 ) ) ;
#4162 = FACE_OUTER_BOUND ( 'NONE', #12940, .T. ) ;
#4163 = DIRECTION ( 'NONE',  ( -1.000000000000000000, 0.000000000000000000, 0.000000000000000000 ) ) ;
#4164 = DIRECTION ( 'NONE',  ( 1.000000000000000000, 0.000000000000000000, 0.000000000000000000 ) ) ;
#4165 = CARTESIAN_POINT ( 'NONE',  ( -66.70000000109246230, 9.143825827087049163, 17.06698730000000097 ) ) ;
#4166 = DIRECTION ( 'NONE',  ( 0.000000000000000000, 0.000000000000000000, -1.000000000000000000 ) ) ;
#4167 = ORIENTED_EDGE ( 'NONE', *, *, #17014, .F. ) ;
#4168 = CARTESIAN_POINT ( 'NONE',  ( 1.656854249492384135, -3.999999999999999112, 12.31250000000001066 ) ) ;
#4169 = CARTESIAN_POINT ( 'NONE',  ( -1.800000000000000711, 0.000000000000000000, 0.000000000000000000 ) ) ;
#4170 = AXIS2_PLACEMENT_3D ( 'NONE', #10797, #8516, #12470 ) ;
#4171 = ORIENTED_EDGE ( 'NONE', *, *, #14972, .F. ) ;
#4172 = CIRCLE ( 'NONE', #6478, 4.000000000000001776 ) ;
#4173 = FACE_OUTER_BOUND ( 'NONE', #11783, .T. ) ;
#4174 = DIRECTION ( 'NONE',  ( 1.000000000000000000, 0.000000000000000000, 0.000000000000000000 ) ) ;
#4175 = CARTESIAN_POINT ( 'NONE',  ( -3.999999999999998224, -1.656854249492383024, 11.18750000273119660 ) ) ;
#4176 = CYLINDRICAL_SURFACE ( 'NONE', #3357, 4.000000000000000000 ) ;
#4177 = VERTEX_POINT ( 'NONE', #7659 ) ;
#4178 = CARTESIAN_POINT ( 'NONE',  ( 2.149474931388133836, 6.264553569211845918, -0.05533025579362121221 ) ) ;
#4179 = EDGE_LOOP ( 'NONE', ( #6639, #21174, #6491, #14240 ) ) ;
#4180 = PRODUCT_DEFINITION_FORMATION_WITH_SPECIFIED_SOURCE ( 'ANY', '', #15290, .NOT_KNOWN. ) ;
#4181 =( GEOMETRIC_REPRESENTATION_CONTEXT ( 3 ) GLOBAL_UNCERTAINTY_ASSIGNED_CONTEXT ( ( #11724 ) ) GLOBAL_UNIT_ASSIGNED_CONTEXT ( ( #11029, #894, #3051 ) ) REPRESENTATION_CONTEXT ( 'NONE', 'WORKASPACE' ) );
#4182 = CARTESIAN_POINT ( 'NONE',  ( 0.000000000000000000, 0.000000000000000000, 19.04999999999996874 ) ) ;
#4183 = CIRCLE ( 'NONE', #8777, 6.000000000000021316 ) ;
#4184 = CARTESIAN_POINT ( 'NONE',  ( -3.999999999999999112, 0.000000000000000000, 13.00000000000001066 ) ) ;
#4185 = CARTESIAN_POINT ( 'NONE',  ( 3.860127959283449428, -8.974600000000002353, 5.000000000000079936 ) ) ;
#4186 = DIRECTION ( 'NONE',  ( -1.000000000000000000, -7.703719777548943412E-32, 0.000000000000000000 ) ) ;
#4187 =( BOUNDED_CURVE ( )  B_SPLINE_CURVE ( 2, ( #21522, #12113, #19733, #6701, #15819, #23091, #17952, #14016, #4900 ),
 .UNSPECIFIED., .F., .F. ) 
 B_SPLINE_CURVE_WITH_KNOTS ( ( 3, 2, 2, 2, 3 ),
 ( 0.6500000000000000222, 0.6624999999999999778, 0.6750000000000000444, 0.6875000000000000000, 0.6999999999999999556 ),
 .UNSPECIFIED. ) 
 CURVE ( )  GEOMETRIC_REPRESENTATION_ITEM ( )  RATIONAL_B_SPLINE_CURVE ( ( 1.000000000000000000, 0.9238795325112867385, 1.000000000000000000, 0.9238795325112867385, 1.000000000000000000, 0.9238795325112867385, 1.000000000000000000, 0.9238795325112867385, 1.000000000000000000 ) ) 
 REPRESENTATION_ITEM ( '' )  );
#4188 = DIRECTION ( 'NONE',  ( 1.000000000000000000, 0.000000000000000000, 0.000000000000000000 ) ) ;
#4189 = CARTESIAN_POINT ( 'NONE',  ( 72.10000000109246798, 12.06698729999999919, 15.85617417291294196 ) ) ;
#4190 = AXIS2_PLACEMENT_3D ( 'NONE', #7911, #16772, #4186 ) ;
#4191 = ORIENTED_EDGE ( 'NONE', *, *, #14406, .F. ) ;
#4192 = VECTOR ( 'NONE', #9666, 1000.000000000000000 ) ;
#4193 = CARTESIAN_POINT ( 'NONE',  ( 4.999999999999999112, 4.057423117305393845, 8.475820894092990443 ) ) ;
#4194 = CARTESIAN_POINT ( 'NONE',  ( -27.50000000000000711, 7.500000000000002665, -33.66025403784446723 ) ) ;
#4195 = CARTESIAN_POINT ( 'NONE',  ( 66.05000000109247082, 9.999999999999998224, 12.93301269999999192 ) ) ;
#4196 = CARTESIAN_POINT ( 'NONE',  ( 2.445694354108821411, 2.445694354108820523, 15.06250000136560452 ) ) ;
#4197 = FACE_OUTER_BOUND ( 'NONE', #14096, .T. ) ;
#4198 = CARTESIAN_POINT ( 'NONE',  ( -2.117863837641485618E-16, 3.458734125000000770, -1.262499998634402765 ) ) ;
#4199 = MECHANICAL_DESIGN_GEOMETRIC_PRESENTATION_REPRESENTATION (  '', ( #6119 ), #7279 ) ;
#4200 = CARTESIAN_POINT ( 'NONE',  ( -4.000000000000000888, 1.656854249492380804, 2.237500000000001599 ) ) ;
#4201 = DIRECTION ( 'NONE',  ( 0.000000000000000000, 0.000000000000000000, -1.000000000000000000 ) ) ;
#4202 = CARTESIAN_POINT ( 'NONE',  ( -2.445694354108818303, -2.445694354108820523, 11.56250000136560629 ) ) ;
#4203 = CARTESIAN_POINT ( 'NONE',  ( 1.546713180332750293, -11.25000000000000355, 10.00000000000008882 ) ) ;
#4204 = ORIENTED_EDGE ( 'NONE', *, *, #445, .T. ) ;
#4205 = EDGE_CURVE ( 'NONE', #4668, #13655, #21195, .T. ) ;
#4206 = CARTESIAN_POINT ( 'NONE',  ( -67.45000000109246230, 7.933012699999995476, 14.99999999999999645 ) ) ;
#4207 = ORIENTED_EDGE ( 'NONE', *, *, #6324, .T. ) ;
#4208 = CARTESIAN_POINT ( 'NONE',  ( 57.93750000000000000, 10.00000000000001776, 18.99999999999999645 ) ) ;
#4209 = CARTESIAN_POINT ( 'NONE',  ( -70.55000000109245661, 11.46158073645647235, 16.46158073645647235 ) ) ;
#4210 = SHAPE_DEFINITION_REPRESENTATION ( #20786, #6707 ) ;
#4211 = VERTEX_POINT ( 'NONE', #8249 ) ;
#4212 = CARTESIAN_POINT ( 'NONE',  ( 65.75000000109245946, 9.999999999999998224, 17.06698730000000097 ) ) ;
#4213 = ORIENTED_EDGE ( 'NONE', *, *, #3827, .T. ) ;
#4214 = CIRCLE ( 'NONE', #15282, 4.000000000000000000 ) ;
#4215 = AXIS2_PLACEMENT_3D ( 'NONE', #13730, #6651, #12171 ) ;
#4216 = ORIENTED_EDGE ( 'NONE', *, *, #9504, .T. ) ;
#4217 = CARTESIAN_POINT ( 'NONE',  ( 3.458734125000001658, 1.432654583217640498, 16.25000000136560629 ) ) ;
#4218 = EDGE_CURVE ( 'NONE', #20787, #12158, #17467, .T. ) ;
#4219 = CARTESIAN_POINT ( 'NONE',  ( 53.25000000000000711, 7.878679656440361612, 17.12132034355964549 ) ) ;
#4220 = AXIS2_PLACEMENT_3D ( 'NONE', #14829, #22083, #300 ) ;
#4221 = CARTESIAN_POINT ( 'NONE',  ( -67.45000000109246230, 7.933012699999995476, 14.99999999999999645 ) ) ;
#4222 = CIRCLE ( 'NONE', #8450, 4.000000000000001776 ) ;
#4223 = CARTESIAN_POINT ( 'NONE',  ( 69.30000000109247082, 10.85617417291294551, 12.93301269999999192 ) ) ;
#4224 = CARTESIAN_POINT ( 'NONE',  ( -72.50000000000000000, 9.999999999999998224, 17.49999999999999645 ) ) ;
#4225 = FACE_OUTER_BOUND ( 'NONE', #847, .T. ) ;
#4226 = CARTESIAN_POINT ( 'NONE',  ( 54.71643183416158251, 12.97181229448535689, 16.31069182806490758 ) ) ;
#4227 = DIRECTION ( 'NONE',  ( -1.000000000000000000, 0.000000000000000000, -0.000000000000000000 ) ) ;
#4228 = CARTESIAN_POINT ( 'NONE',  ( 1.432654583217640276, 3.458734125000000770, 2.675000001365597679 ) ) ;
#4229 = CARTESIAN_POINT ( 'NONE',  ( -1.432654583217638944, 3.458734125000000326, 10.25000000136560629 ) ) ;
#4230 = CARTESIAN_POINT ( 'NONE',  ( -1.656854249492379250, 4.000000000000000000, 16.93750000273119838 ) ) ;
#4231 = CARTESIAN_POINT ( 'NONE',  ( -90.00000000000000000, 0.000000000000000000, 0.000000000000000000 ) ) ;
#4232 = VECTOR ( 'NONE', #23050, 1000.000000000000114 ) ;
#4233 = VERTEX_POINT ( 'NONE', #11509 ) ;
#4234 = ADVANCED_FACE ( 'NONE', ( #16990 ), #6206, .T. ) ;
#4235 = DIRECTION ( 'NONE',  ( 0.000000000000000000, -0.5877852522924624790, -0.8090169943749553338 ) ) ;
#4236 = ORIENTED_EDGE ( 'NONE', *, *, #17941, .F. ) ;
#4237 = CARTESIAN_POINT ( 'NONE',  ( 57.43518183416157541, 9.931948859054372747, 17.99999999999999645 ) ) ;
#4239 = CIRCLE ( 'NONE', #21818, 4.000000000000000000 ) ;
#4238 = FILL_AREA_STYLE ('',( #13243 ) ) ;
#4240 = CARTESIAN_POINT ( 'NONE',  ( -3.458734125000000326, 0.000000000000000000, 3.737500001365594571 ) ) ;
#4241 = ADVANCED_FACE ( 'NONE', ( #4639 ), #20680, .F. ) ;
#4242 = DIRECTION ( 'NONE',  ( 0.000000000000000000, 0.000000000000000000, -1.000000000000000000 ) ) ;
#4243 = ORIENTED_EDGE ( 'NONE', *, *, #5123, .F. ) ;
#4244 = CARTESIAN_POINT ( 'NONE',  ( 4.000000000000000888, 4.898587196589412829E-16, 14.50000000000001066 ) ) ;
#4245 = CARTESIAN_POINT ( 'NONE',  ( 0.2500000000000002220, 0.000000000000000000, 0.000000000000000000 ) ) ;
#4246 = DIRECTION ( 'NONE',  ( -1.224646799147353207E-16, 0.000000000000000000, -1.000000000000000000 ) ) ;
#4247 = VERTEX_POINT ( 'NONE', #4399 ) ;
#4248 = EDGE_CURVE ( 'NONE', #19691, #14136, #6401, .T. ) ;
#4249 = EDGE_CURVE ( 'NONE', #21235, #16763, #6152, .T. ) ;
#4250 = CARTESIAN_POINT ( 'NONE',  ( -70.05000000218494449, 12.50000000000000000, 16.03553390593273420 ) ) ;
#4251 = LINE ( 'NONE', #995, #6024 ) ;
#4252 = VECTOR ( 'NONE', #9808, 1000.000000000000000 ) ;
#4253 = LINE ( 'NONE', #22566, #12224 ) ;
#4254 = CARTESIAN_POINT ( 'NONE',  ( 4.999999999999999112, -9.241976615262146311, -1.699438267350473097 ) ) ;
#4255 = LINE ( 'NONE', #11589, #15455 ) ;
#4256 = LINE ( 'NONE', #22574, #20615 ) ;
#4257 = CARTESIAN_POINT ( 'NONE',  ( 57.31481816583843170, 12.99999999999999822, 14.93194885905435676 ) ) ;
#4258 = CARTESIAN_POINT ( 'NONE',  ( -2.445694354108819635, -2.445694354108820967, 4.112500001365594571 ) ) ;
#4259 = CARTESIAN_POINT ( 'NONE',  ( -2.445694354108819191, 2.445694354108820523, 15.56250000136560629 ) ) ;
#4260 = CARTESIAN_POINT ( 'NONE',  ( -71.89999999999999147, 7.499999999999996447, 14.99999999999999645 ) ) ;
#4261 = CARTESIAN_POINT ( 'NONE',  ( -72.15000000109246514, 11.46158073645647235, 16.46158073645647235 ) ) ;
#4262 = CARTESIAN_POINT ( 'NONE',  ( 4.000000000000000000, 4.898587196589412829E-16, -2.199999999999998845 ) ) ;
#4263 = VERTEX_POINT ( 'NONE', #13355 ) ;
#4264 = CARTESIAN_POINT ( 'NONE',  ( -3.522875095019672109, 2.820352903225427532, -3.598441714920591394 ) ) ;
#4265 = DIRECTION ( 'NONE',  ( -1.000000000000000000, -0.000000000000000000, -0.000000000000000000 ) ) ;
#4266 = EDGE_CURVE ( 'NONE', #22700, #15024, #5423, .T. ) ;
#4267 = CARTESIAN_POINT ( 'NONE',  ( -69.85000000109248219, 7.933012699999995476, 14.99999999999999645 ) ) ;
#4268 = ORIENTED_EDGE ( 'NONE', *, *, #9067, .T. ) ;
#4269 = ORIENTED_EDGE ( 'NONE', *, *, #19420, .T. ) ;
#4270 = CARTESIAN_POINT ( 'NONE',  ( 34.99999999999999289, 4.500000000000009770, -50.00000000000000711 ) ) ;
#4271 = CARTESIAN_POINT ( 'NONE',  ( 52.12500000000000711, 12.82842712474620228, 17.82842712474617386 ) ) ;
#4272 = ORIENTED_EDGE ( 'NONE', *, *, #22533, .F. ) ;
#4273 = CARTESIAN_POINT ( 'NONE',  ( 1.243802165048773611, -3.900692638707475624, -3.223146290109810241 ) ) ;
#4274 = EDGE_CURVE ( 'NONE', #7229, #9962, #17050, .T. ) ;
#4275 = UNCERTAINTY_MEASURE_WITH_UNIT (LENGTH_MEASURE( 1.000000000000000082E-05 ), #10865, 'distance_accuracy_value', 'NONE');
#4276 = CARTESIAN_POINT ( 'NONE',  ( 68.95000000109247651, 8.538419263543522320, 16.46158073645647235 ) ) ;
#4277 = B_SPLINE_CURVE_WITH_KNOTS ( 'NONE', 3,
 ( #18430, #22007, #2129, #5618, #20568, #1899, #2009, #9464 ),
 .UNSPECIFIED., .F., .F.,
 ( 4, 2, 2, 4 ),
 ( 7.780516681398759253E-20, 0.002450665683189819696, 0.003675998524784729327, 0.004901331366379639391 ),
 .UNSPECIFIED. ) ;
#4278 = CARTESIAN_POINT ( 'NONE',  ( 2.828427124746192067, -2.828427124746189847, 19.37500000000001066 ) ) ;
#4279 = CARTESIAN_POINT ( 'NONE',  ( 71.10000000109246798, 10.85617417291294551, 12.93301269999999370 ) ) ;
#4280 = ORIENTED_EDGE ( 'NONE', *, *, #11223, .F. ) ;
#4281 = FACE_BOUND ( 'NONE', #2290, .T. ) ;
#4282 = CARTESIAN_POINT ( 'NONE',  ( 55.96875000000000000, 5.999999999999987566, 13.34314575050763452 ) ) ;
#4283 = B_SPLINE_CURVE_WITH_KNOTS ( 'NONE', 3,
 ( #3330, #9227, #7421, #14617, #5605, #12593, #20195, #10674 ),
 .UNSPECIFIED., .F., .F.,
 ( 4, 2, 2, 4 ),
 ( 0.000000000000000000, 0.002450665683189820997, 0.003675998524784731495, 0.004901331366379641993 ),
 .UNSPECIFIED. ) ;
#4284 = DIRECTION ( 'NONE',  ( 1.000000000000000000, 7.703719777548943412E-32, 0.000000000000000000 ) ) ;
#4285 = CARTESIAN_POINT ( 'NONE',  ( 2.445694354108821411, 2.445694354108820523, 18.06250000136560274 ) ) ;
#4286 = LINE ( 'NONE', #22471, #965 ) ;
#4287 = CARTESIAN_POINT ( 'NONE',  ( -2.828427124746189403, -2.828427124746190735, 0.4250000000000017653 ) ) ;
#4288 = VERTEX_POINT ( 'NONE', #20737 ) ;
#4289 = DIRECTION ( 'NONE',  ( -1.000000000000000000, -0.000000000000000000, -0.000000000000000000 ) ) ;
#4290 = VERTEX_POINT ( 'NONE', #11680 ) ;
#4291 = FACE_OUTER_BOUND ( 'NONE', #2155, .T. ) ;
#4292 = DIRECTION ( 'NONE',  ( -0.000000000000000000, 0.000000000000000000, -1.000000000000000000 ) ) ;
#4293 = ORIENTED_EDGE ( 'NONE', *, *, #10128, .T. ) ;
#4294 = CARTESIAN_POINT ( 'NONE',  ( 69.00000000218494733, 9.999999999999998224, 12.49999999999999289 ) ) ;
#4295 = CARTESIAN_POINT ( 'NONE',  ( 9.920644283265380691E-16, 4.000000000000000000, 14.87500000273119660 ) ) ;
#4296 = CARTESIAN_POINT ( 'NONE',  ( -60.00000000000000711, -10.00000000000000178, 14.99999999999999467 ) ) ;
#4297 = AXIS2_PLACEMENT_3D ( 'NONE', #6212, #2369, #13295 ) ;
#4298 = EDGE_CURVE ( 'NONE', #4468, #19953, #15038, .T. ) ;
#4299 = CARTESIAN_POINT ( 'NONE',  ( -0.3649867057748917842, 3.983313282257320509, 9.889028792932920808 ) ) ;
#4300 = EDGE_LOOP ( 'NONE', ( #22034, #7914, #18353, #8052 ) ) ;
#4301 = DIRECTION ( 'NONE',  ( 0.000000000000000000, 0.000000000000000000, 1.000000000000000000 ) ) ;
#4302 = ORIENTED_EDGE ( 'NONE', *, *, #15990, .F. ) ;
#4303 = CARTESIAN_POINT ( 'NONE',  ( 71.25000000109248788, 9.999999999999998224, 17.06698730000000097 ) ) ;
#4304 = CARTESIAN_POINT ( 'NONE',  ( 4.000000000000001776, -1.656854249492379694, 13.43750000000001243 ) ) ;
#4305 = DIRECTION ( 'NONE',  ( 0.000000000000000000, 0.000000000000000000, 1.000000000000000000 ) ) ;
#4306 = VERTEX_POINT ( 'NONE', #5347 ) ;
#4307 = CARTESIAN_POINT ( 'NONE',  ( 2.000000000000001776, 0.000000000000000000, -8.073750000000021743 ) ) ;
#4308 = CARTESIAN_POINT ( 'NONE',  ( 70.85000000109246798, 7.933012699999995476, 14.99999999999999645 ) ) ;
#4309 = EDGE_LOOP ( 'NONE', ( #377, #15317, #1292, #15349, #4884 ) ) ;
#4310 = CARTESIAN_POINT ( 'NONE',  ( -35.00000000000000711, 4.500000000000003553, -49.99999999999999289 ) ) ;
#4311 = DIRECTION ( 'NONE',  ( -0.000000000000000000, 1.000000000000000000, -0.000000000000000000 ) ) ;
#4312 = CARTESIAN_POINT ( 'NONE',  ( 68.60000000109246798, 9.143825827087050939, 12.93301269999999370 ) ) ;
#4313 = CARTESIAN_POINT ( 'NONE',  ( -3.458734124999998993, 1.432654583217640276, 15.37500000136560807 ) ) ;
#4314 = DIRECTION ( 'NONE',  ( -1.000000000000000000, 0.000000000000000000, 0.000000000000000000 ) ) ;
#4315 = LINE ( 'NONE', #13674, #2707 ) ;
#4316 = CARTESIAN_POINT ( 'NONE',  ( 1.656854249492380360, 4.000000000000000000, 2.987500000000002487 ) ) ;
#4317 = CARTESIAN_POINT ( 'NONE',  ( -4.000000000000000000, 0.000000000000000000, -3.574999997268813345 ) ) ;
#4318 = CARTESIAN_POINT ( 'NONE',  ( -35.00000000000000711, 1.500000000000003109, -49.99999999999999289 ) ) ;
#4319 = CARTESIAN_POINT ( 'NONE',  ( -90.00000000000000000, 8.247996192257451316E-16, 6.735000000000022524 ) ) ;
#4320 = EDGE_LOOP ( 'NONE', ( #18287, #12181, #1445, #1390 ) ) ;
#4321 = CARTESIAN_POINT ( 'NONE',  ( 50.38765154071656838, -8.974600000000002353, 5.000000000000079936 ) ) ;
#4322 = ORIENTED_EDGE ( 'NONE', *, *, #2574, .F. ) ;
#4323 = CARTESIAN_POINT ( 'NONE',  ( 55.50000000000000711, 12.82842712474617741, 12.17157287525379239 ) ) ;
#4324 = CARTESIAN_POINT ( 'NONE',  ( -67.25000000109245946, 12.06698730000000097, 14.99999999999999645 ) ) ;
#4325 = ITEM_DEFINED_TRANSFORMATION ( 'NONE', 'NONE', #6099,  #7318 ) ;
#4326 = VERTEX_POINT ( 'NONE', #13119 ) ;
#4327 = CARTESIAN_POINT ( 'NONE',  ( 4.999999999999999112, -8.461683424509331530, 2.223716399045538861 ) ) ;
#4328 = ORIENTED_EDGE ( 'NONE', *, *, #21516, .F. ) ;
#4329 = ORIENTED_EDGE ( 'NONE', *, *, #21331, .T. ) ;
#4330 = CARTESIAN_POINT ( 'NONE',  ( -2.445694354108819191, 2.445694354108820523, 17.56250000136560274 ) ) ;
#4331 = CARTESIAN_POINT ( 'NONE',  ( 55.78125000000000000, 8.757359312880703683, 11.99999999999999822 ) ) ;
#4332 = CARTESIAN_POINT ( 'NONE',  ( -66.25000000109247367, 12.06698730000000097, 14.99999999999999645 ) ) ;
#4333 = VECTOR ( 'NONE', #12410, 1000.000000000000000 ) ;
#4334 = CARTESIAN_POINT ( 'NONE',  ( 70.65000000109247935, 7.933012699999995476, 14.99999999999999645 ) ) ;
#4335 = EDGE_CURVE ( 'NONE', #8665, #2584, #13235, .T. ) ;
#4336 = CARTESIAN_POINT ( 'NONE',  ( -66.15000000109247935, 8.538419263543524096, 13.53841926354352054 ) ) ;
#4337 = CARTESIAN_POINT ( 'NONE',  ( 3.250000000000002665, -5.629165124598850767, -3.700000000000000178 ) ) ;
#4338 = CARTESIAN_POINT ( 'NONE',  ( 59.68518183416157541, 10.06805114094562548, 11.99999999999999645 ) ) ;
#4339 = CARTESIAN_POINT ( 'NONE',  ( 60.00000000000000000, 12.92210812677098275, 14.19519413938285268 ) ) ;
#4340 = CARTESIAN_POINT ( 'NONE',  ( 3.458734125000001214, -1.432654583217639610, 5.425000001365595459 ) ) ;
#4341 = CARTESIAN_POINT ( 'NONE',  ( -6.161016159283438931, -8.974600000000002353, 5.000000000000079936 ) ) ;
#4342 = CARTESIAN_POINT ( 'NONE',  ( 4.000000000000000888, 4.898587196589412829E-16, 13.62500000273119660 ) ) ;
#4343 = EDGE_CURVE ( 'NONE', #8977, #9649, #975, .T. ) ;
#4344 = DIRECTION ( 'NONE',  ( -1.000000000000000000, 0.000000000000000000, 0.000000000000000000 ) ) ;
#4345 = VECTOR ( 'NONE', #14591, 1000.000000000000000 ) ;
#4346 = ORIENTED_EDGE ( 'NONE', *, *, #11430, .F. ) ;
#4347 = CARTESIAN_POINT ( 'NONE',  ( -2.762848947613220307, 4.746226468750993632, 10.00000000000000888 ) ) ;
#4348 = ORIENTED_EDGE ( 'NONE', *, *, #20475, .T. ) ;
#4349 = CARTESIAN_POINT ( 'NONE',  ( 60.43518183416157541, 9.931948859054372747, 17.99999999999999645 ) ) ;
#4350 = SURFACE_STYLE_USAGE ( .BOTH. , #23521 ) ;
#4351 = CARTESIAN_POINT ( 'NONE',  ( 2.445694354108820523, -2.445694354108820079, 1.112500001365595681 ) ) ;
#4352 = CARTESIAN_POINT ( 'NONE',  ( -3.458734125000000326, 0.000000000000000000, 0.7375000013655954589 ) ) ;
#4353 = EDGE_LOOP ( 'NONE', ( #1248, #1184 ) ) ;
#4354 = CARTESIAN_POINT ( 'NONE',  ( -3.999999999999999112, 0.000000000000000000, 12.00000000000001066 ) ) ;
#4355 = PRESENTATION_STYLE_ASSIGNMENT (( #13598 ) ) ;
#4356 = LINE ( 'NONE', #13489, #11041 ) ;
#4357 = EDGE_LOOP ( 'NONE', ( #14455, #4782, #19653, #9352 ) ) ;
#4358 = PRODUCT_DEFINITION_SHAPE ( 'NONE', 'NONE',  #23699 ) ;
#4359 = CARTESIAN_POINT ( 'NONE',  ( -71.75000000218496155, 11.03553390593273598, 17.50000000000000355 ) ) ;
#4360 = CARTESIAN_POINT ( 'NONE',  ( 2.445694354108820079, 2.445694354108820523, -2.387499998634403653 ) ) ;
#4361 = EDGE_CURVE ( 'NONE', #10070, #9347, #6267, .T. ) ;
#4362 = FACE_OUTER_BOUND ( 'NONE', #7081, .T. ) ;
#4363 = CARTESIAN_POINT ( 'NONE',  ( 1.432654583217643163, -3.458734124999999882, 18.00000000136560274 ) ) ;
#4364 = EDGE_CURVE ( 'NONE', #22188, #9402, #20851, .T. ) ;
#4365 = DIRECTION ( 'NONE',  ( 0.3420201433256622181, 0.9396926207859107594, -6.162975822039141593E-32 ) ) ;
#4366 = CARTESIAN_POINT ( 'NONE',  ( 70.60000000109246798, 7.933012699999995476, 15.85617417291294196 ) ) ;
#4367 = DIRECTION ( 'NONE',  ( -1.000000000000000000, -0.000000000000000000, 0.000000000000000000 ) ) ;
#4368 = CARTESIAN_POINT ( 'NONE',  ( 56.56481816583843170, 6.999999999999998224, 15.06805114094563436 ) ) ;
#4369 = CARTESIAN_POINT ( 'NONE',  ( 1.432654583217640276, 3.458734125000000770, 3.675000001365597235 ) ) ;
#4370 = CARTESIAN_POINT ( 'NONE',  ( 3.458734125000002546, -1.432654583217639610, 12.12500000136560629 ) ) ;
#4371 = ADVANCED_FACE ( 'NONE', ( #12269 ), #4458, .T. ) ;
#4372 = DIRECTION ( 'NONE',  ( 0.000000000000000000, 0.000000000000000000, -1.000000000000000000 ) ) ;
#4373 = CARTESIAN_POINT ( 'NONE',  ( 20.39626908033275043, -11.25000000000000355, 5.000000000000079936 ) ) ;
#4374 = LINE ( 'NONE', #20321, #18115 ) ;
#4375 = CARTESIAN_POINT ( 'NONE',  ( 14.99999999999999645, 10.00000000000000000, -20.00000000000000355 ) ) ;
#4376 = VERTEX_POINT ( 'NONE', #3132 ) ;
#4377 = CARTESIAN_POINT ( 'NONE',  ( -3.436319922987618902, 2.634841920961291439, -3.531542292955721862 ) ) ;
#4378 = CIRCLE ( 'NONE', #22784, 6.000000000000000888 ) ;
#4379 = CARTESIAN_POINT ( 'NONE',  ( -4.000000000000000888, 1.656854249492380804, 4.362500002731187543 ) ) ;
#4380 = CARTESIAN_POINT ( 'NONE',  ( -72.05000000109247082, 9.999999999999998224, 17.06698730000000097 ) ) ;
#4381 = ORIENTED_EDGE ( 'NONE', *, *, #3759, .F. ) ;
#4382 = ORIENTED_EDGE ( 'NONE', *, *, #8196, .F. ) ;
#4383 = CARTESIAN_POINT ( 'NONE',  ( -2.688821387764050996E-14, -4.618802153517012954, -0.4999999999999995559 ) ) ;
#4384 = CARTESIAN_POINT ( 'NONE',  ( 47.84242505928347100, -8.974600000000002353, 5.000000000000079936 ) ) ;
#4385 = ORIENTED_EDGE ( 'NONE', *, *, #8180, .T. ) ;
#4386 = DIRECTION ( 'NONE',  ( 0.000000000000000000, 0.000000000000000000, -1.000000000000000000 ) ) ;
#4387 = EDGE_CURVE ( 'NONE', #18254, #23165, #11920, .T. ) ;
#4388 = CARTESIAN_POINT ( 'NONE',  ( 67.50000000109247367, 7.933012699999995476, 14.14382582708705094 ) ) ;
#4389 = VECTOR ( 'NONE', #9008, 1000.000000000000000 ) ;
#4390 = VECTOR ( 'NONE', #3745, 1000.000000000000000 ) ;
#4391 = CARTESIAN_POINT ( 'NONE',  ( 67.30000000109247082, 12.06698730000000275, 15.85617417291294196 ) ) ;
#4392 = EDGE_CURVE ( 'NONE', #21422, #18582, #7946, .T. ) ;
#4393 = AXIS2_PLACEMENT_3D ( 'NONE', #3682, #7538, #13062 ) ;
#4394 = ORIENTED_EDGE ( 'NONE', *, *, #21186, .T. ) ;
#4395 = LINE ( 'NONE', #18778, #11864 ) ;
#4396 = CARTESIAN_POINT ( 'NONE',  ( 57.56250000000000000, 5.999999999999996447, 15.00000000000001599 ) ) ;
#4397 = CARTESIAN_POINT ( 'NONE',  ( -3.999999999999999112, 0.000000000000000000, 12.12500000273119838 ) ) ;
#4398 = EDGE_CURVE ( 'NONE', #20854, #5860, #858, .T. ) ;
#4399 = CARTESIAN_POINT ( 'NONE',  ( 65.65000000109247935, 9.999999999999998224, 17.06698730000000097 ) ) ;
#4400 = LINE ( 'NONE', #16749, #21963 ) ;
#4401 = EDGE_CURVE ( 'NONE', #5267, #19658, #5133, .T. ) ;
#4402 = DIRECTION ( 'NONE',  ( -7.087422195345011518E-32, -1.000000000000000000, 0.000000000000000000 ) ) ;
#4403 = ORIENTED_EDGE ( 'NONE', *, *, #6589, .T. ) ;
#4404 = CARTESIAN_POINT ( 'NONE',  ( 4.999999999999999112, 5.538577986808997267, -6.772677083992326708 ) ) ;
#4405 = CARTESIAN_POINT ( 'NONE',  ( 4.000000000000000000, 4.898587196589412829E-16, 1.925000002731188209 ) ) ;
#4406 = CARTESIAN_POINT ( 'NONE',  ( -70.64999999999999147, 12.50000000000000000, 13.96446609406725692 ) ) ;
#4407 = ORIENTED_EDGE ( 'NONE', *, *, #14868, .T. ) ;
#4408 = FACE_OUTER_BOUND ( 'NONE', #18514, .T. ) ;
#4409 = CARTESIAN_POINT ( 'NONE',  ( 4.999999999999999112, -0.4999240074895051067, 8.734705317681624948 ) ) ;
#4410 = DIRECTION ( 'NONE',  ( -1.000000000000000000, 0.000000000000000000, 0.000000000000000000 ) ) ;
#4411 = AXIS2_PLACEMENT_3D ( 'NONE', #3224, #14153, #12484 ) ;
#4412 = VECTOR ( 'NONE', #5222, 1000.000000000000000 ) ;
#4413 = CARTESIAN_POINT ( 'NONE',  ( 0.000000000000000000, 0.000000000000000000, 0.000000000000000000 ) ) ;
#4414 = ORIENTED_EDGE ( 'NONE', *, *, #21485, .T. ) ;
#4415 = PLANE ( 'NONE',  #14523 ) ;
#4416 = ORIENTED_EDGE ( 'NONE', *, *, #22909, .T. ) ;
#4417 = CARTESIAN_POINT ( 'NONE',  ( 14.99999999999995559, 15.00000000000000000, -50.00000000000000000 ) ) ;
#4418 = DIRECTION ( 'NONE',  ( -1.224646799147353207E-16, 0.000000000000000000, -1.000000000000000000 ) ) ;
#4419 = DIRECTION ( 'NONE',  ( 0.3420201433256622181, -0.9396926207859107594, 0.000000000000000000 ) ) ;
#4420 = VERTEX_POINT ( 'NONE', #10473 ) ;
#4421 = CARTESIAN_POINT ( 'NONE',  ( 35.00000000000000000, 4.500000000000001776, -20.00000000000000355 ) ) ;
#4422 = DIRECTION ( 'NONE',  ( 0.000000000000000000, 0.000000000000000000, -1.000000000000000000 ) ) ;
#4423 = CARTESIAN_POINT ( 'NONE',  ( 69.90000000109246514, 9.143825827087049163, 17.06698730000000097 ) ) ;
#4424 = ORIENTED_EDGE ( 'NONE', *, *, #19916, .T. ) ;
#4425 = AXIS2_PLACEMENT_3D ( 'NONE', #20389, #22306, #14933 ) ;
#4426 = DIRECTION ( 'NONE',  ( -1.000000000000000000, -0.000000000000000000, -0.000000000000000000 ) ) ;
#4427 = CIRCLE ( 'NONE', #14003, 11.00000000000000000 ) ;
#4428 = CARTESIAN_POINT ( 'NONE',  ( 2.828427124746192067, -2.828427124746189847, 10.50000000273119660 ) ) ;
#4429 = EDGE_CURVE ( 'NONE', #2372, #15450, #8304, .T. ) ;
#4430 = CARTESIAN_POINT ( 'NONE',  ( 71.50000000109247367, 9.143825827087049163, 17.06698729999999742 ) ) ;
#4431 = CARTESIAN_POINT ( 'NONE',  ( 1.432654583217641164, 3.458734125000000326, 15.12500000136560807 ) ) ;
#4432 = DIRECTION ( 'NONE',  ( -1.000000000000000000, 0.000000000000000000, 0.000000000000000000 ) ) ;
#4433 = EDGE_CURVE ( 'NONE', #14063, #1063, #153, .T. ) ;
#4434 = DIRECTION ( 'NONE',  ( 7.087422195345011518E-32, 1.000000000000000000, -0.000000000000000000 ) ) ;
#4435 = ORIENTED_EDGE ( 'NONE', *, *, #15774, .F. ) ;
#4436 = CARTESIAN_POINT ( 'NONE',  ( -2.828427124746190291, 2.828427124746190291, 1.175000000000000711 ) ) ;
#4437 = DIRECTION ( 'NONE',  ( 1.000000000000000000, 0.000000000000000000, 0.000000000000000000 ) ) ;
#4438 = DIRECTION ( 'NONE',  ( -1.000000000000000000, -7.703719777548943412E-32, 0.000000000000000000 ) ) ;
#4439 = LINE ( 'NONE', #6600, #11912 ) ;
#4440 = ORIENTED_EDGE ( 'NONE', *, *, #17941, .T. ) ;
#4441 = CARTESIAN_POINT ( 'NONE',  ( -65.75000000109247367, 8.538419263543522320, 16.46158073645647235 ) ) ;
#4442 = ORIENTED_EDGE ( 'NONE', *, *, #9095, .F. ) ;
#4443 = CARTESIAN_POINT ( 'NONE',  ( -67.95000000109247651, 11.46158073645647235, 13.53841926354352232 ) ) ;
#4444 = ITEM_DEFINED_TRANSFORMATION ( 'NONE', 'NONE', #2653,  #7318 ) ;
#4445 = ORIENTED_EDGE ( 'NONE', *, *, #23101, .T. ) ;
#4446 = DIRECTION ( 'NONE',  ( 1.000000000000000000, 0.000000000000000000, 0.000000000000000000 ) ) ;
#4447 = ORIENTED_EDGE ( 'NONE', *, *, #15114, .F. ) ;
#4448 = ORIENTED_EDGE ( 'NONE', *, *, #7466, .F. ) ;
#4449 = CARTESIAN_POINT ( 'NONE',  ( 3.458734125000001658, 4.235727675282972223E-16, 17.18750000136560629 ) ) ;
#4450 = CARTESIAN_POINT ( 'NONE',  ( 51.65625000000000711, 7.000000000000003553, 16.24264068711929099 ) ) ;
#4451 = CARTESIAN_POINT ( 'NONE',  ( -66.80000000109247082, 9.143825827087050939, 12.93301269999999370 ) ) ;
#4452 = CARTESIAN_POINT ( 'NONE',  ( 68.60000000109248219, 12.06698729999999919, 14.14382582708705094 ) ) ;
#4453 = CARTESIAN_POINT ( 'NONE',  ( -66.25000000109245946, 9.999999999999998224, 12.93301269999999192 ) ) ;
#4454 = LINE ( 'NONE', #7948, #16407 ) ;
#4455 = CARTESIAN_POINT ( 'NONE',  ( 57.52893183416158962, 11.17458954617365663, 18.02818770551464311 ) ) ;
#4456 = DIRECTION ( 'NONE',  ( 0.000000000000000000, 0.000000000000000000, 1.000000000000000000 ) ) ;
#4457 = CARTESIAN_POINT ( 'NONE',  ( -1.432654583217640498, 3.458734125000000770, 2.800000001365598123 ) ) ;
#4458 = CYLINDRICAL_SURFACE ( 'NONE', #2059, 4.250000000000000000 ) ;
#4459 = CARTESIAN_POINT ( 'NONE',  ( 1.971781867644420635E-15, -4.000000000000000000, 10.37500000273119660 ) ) ;
#4460 = LINE ( 'NONE', #11922, #14191 ) ;
#4461 = EDGE_LOOP ( 'NONE', ( #9468, #19930, #6064, #6579, #12750 ) ) ;
#4462 = CARTESIAN_POINT ( 'NONE',  ( 9.920644283265380691E-16, 4.000000000000000000, 13.75000000000001066 ) ) ;
#4463 = ORIENTED_EDGE ( 'NONE', *, *, #18863, .T. ) ;
#4464 = CARTESIAN_POINT ( 'NONE',  ( 58.74768183416157541, 7.830560233210222876, 17.07320092032950498 ) ) ;
#4465 = CARTESIAN_POINT ( 'NONE',  ( 0.000000000000000000, -19.99999999999999645, 0.000000000000000000 ) ) ;
#4466 = CARTESIAN_POINT ( 'NONE',  ( 3.458734125000000326, 1.432654583217640498, 3.300000001365598568 ) ) ;
#4467 = CARTESIAN_POINT ( 'NONE',  ( 1.432654583217639832, 3.458734125000000326, -0.5749999986344047631 ) ) ;
#4468 = VERTEX_POINT ( 'NONE', #17754 ) ;
#4469 = CARTESIAN_POINT ( 'NONE',  ( 1.971781867644420635E-15, -4.000000000000000000, 14.25000000000001066 ) ) ;
#4470 = EDGE_CURVE ( 'NONE', #19611, #8470, #480, .T. ) ;
#4471 = CARTESIAN_POINT ( 'NONE',  ( 14.99999999999995914, 15.00000000000000000, -20.00000000000000355 ) ) ;
#4472 = CARTESIAN_POINT ( 'NONE',  ( -6.500000000000000000, -3.752776749732573247, -3.119443416399232394 ) ) ;
#4473 = VERTEX_POINT ( 'NONE', #17647 ) ;
#4474 = CARTESIAN_POINT ( 'NONE',  ( -69.85000000218495586, 11.03553390593273598, 12.49999999999999289 ) ) ;
#4475 = CARTESIAN_POINT ( 'NONE',  ( -1.432654583217640498, 3.458734125000000770, -1.199999998634403209 ) ) ;
#4476 = AXIS2_PLACEMENT_3D ( 'NONE', #4006, #286, #169 ) ;
#4477 = DIRECTION ( 'NONE',  ( -1.000000000000000000, 0.000000000000000000, 0.000000000000000000 ) ) ;
#4478 = CARTESIAN_POINT ( 'NONE',  ( 66.49999999999998579, 9.999999999999998224, 12.49999999999999289 ) ) ;
#4479 = CARTESIAN_POINT ( 'NONE',  ( -71.09999999999999432, 7.499999999999996447, 14.99999999999999645 ) ) ;
#4480 = STYLED_ITEM ( 'NONE', ( #18280 ), #6242 ) ;
#4481 = CARTESIAN_POINT ( 'NONE',  ( 70.25000000109247367, 12.06698730000000097, 14.99999999999999645 ) ) ;
#4482 = VECTOR ( 'NONE', #19311, 1000.000000000000114 ) ;
#4483 = DIRECTION ( 'NONE',  ( 1.000000000000000000, 7.703719777548943412E-32, 0.000000000000000000 ) ) ;
#4484 = CARTESIAN_POINT ( 'NONE',  ( 55.53356816583845301, 11.31069182806492712, 17.97181229448534623 ) ) ;
#4485 = CARTESIAN_POINT ( 'NONE',  ( -1.432654583217640498, 3.458734125000000770, 5.800000001365597235 ) ) ;
#4486 = CARTESIAN_POINT ( 'NONE',  ( 1.025207404391860050E-15, 3.458734125000000770, 10.43750000136560629 ) ) ;
#4487 = CARTESIAN_POINT ( 'NONE',  ( 67.54999999999999716, 12.50000000000000000, 16.03553390593273775 ) ) ;
#4488 = CARTESIAN_POINT ( 'NONE',  ( -68.20000000109246230, 10.85617417291294551, 17.06698730000000097 ) ) ;
#4489 = CARTESIAN_POINT ( 'NONE',  ( -70.10000000218494165, 11.76776695296636888, 16.76776695296636532 ) ) ;
#4490 = CARTESIAN_POINT ( 'NONE',  ( -69.79999999999999716, 11.76776695296636888, 13.23223304703362579 ) ) ;
#4491 = ORIENTED_EDGE ( 'NONE', *, *, #16413, .F. ) ;
#4492 = CARTESIAN_POINT ( 'NONE',  ( 60.00000000000000000, 9.999999999999998224, 12.49999999999999289 ) ) ;
#4493 =( LENGTH_UNIT ( ) NAMED_UNIT ( * ) SI_UNIT ( .MILLI., .METRE. ) );
#4494 = CARTESIAN_POINT ( 'NONE',  ( -2.828427124746189403, -2.828427124746190735, 3.550000002731189763 ) ) ;
#4495 = VERTEX_POINT ( 'NONE', #10234 ) ;
#4496 = ORIENTED_EDGE ( 'NONE', *, *, #10595, .F. ) ;
#4497 = AXIS2_PLACEMENT_3D ( 'NONE', #12586, #12816, #1645 ) ;
#4498 = ADVANCED_FACE ( 'NONE', ( #17524 ), #22657, .T. ) ;
#4499 = CARTESIAN_POINT ( 'NONE',  ( -1.656854249492381248, -3.999999999999999112, 1.612500002731187543 ) ) ;
#4500 = ADVANCED_FACE ( 'NONE', ( #4812 ), #3007, .T. ) ;
#4501 = FACE_OUTER_BOUND ( 'NONE', #13165, .T. ) ;
#4502 = VERTEX_POINT ( 'NONE', #23124 ) ;
#4503 = CARTESIAN_POINT ( 'NONE',  ( -0.1750025118121544265, -4.719839900820635314, -3.469254087858253399 ) ) ;
#4504 =( GEOMETRIC_REPRESENTATION_CONTEXT ( 3 ) GLOBAL_UNCERTAINTY_ASSIGNED_CONTEXT ( ( #4275 ) ) GLOBAL_UNIT_ASSIGNED_CONTEXT ( ( #10865, #7140, #7018 ) ) REPRESENTATION_CONTEXT ( 'NONE', 'WORKASPACE' ) );
#4505 = VECTOR ( 'NONE', #2349, 1000.000000000000000 ) ;
#4506 = UNCERTAINTY_MEASURE_WITH_UNIT (LENGTH_MEASURE( 1.000000000000000082E-05 ), #7670, 'distance_accuracy_value', 'NONE');
#4507 = EDGE_CURVE ( 'NONE', #18318, #10729, #6739, .T. ) ;
#4508 = CARTESIAN_POINT ( 'NONE',  ( 67.00000000109247367, 12.06698730000000275, 14.14382582708705094 ) ) ;
#4509 = TOROIDAL_SURFACE ( 'NONE', #9506, 5.479999999999998650, 1.020000000000000018 ) ;
#4510 = CARTESIAN_POINT ( 'NONE',  ( 67.15000000109247935, 11.46158073645647235, 13.53841926354352232 ) ) ;
#4511 = ORIENTED_EDGE ( 'NONE', *, *, #4218, .T. ) ;
#4512 = AXIS2_PLACEMENT_3D ( 'NONE', #6107, #18910, #2498 ) ;
#4513 = CARTESIAN_POINT ( 'NONE',  ( 1.236993788156008760E-15, 0.000000000000000000, 21.31370849898476649 ) ) ;
#4514 = CARTESIAN_POINT ( 'NONE',  ( 55.03125000000000000, 11.65685424949239923, 18.99999999999998934 ) ) ;
#4515 = DIRECTION ( 'NONE',  ( 0.000000000000000000, 0.000000000000000000, -1.000000000000000000 ) ) ;
#4516 = CARTESIAN_POINT ( 'NONE',  ( 3.458734125000002102, -1.432654583217639610, 17.87500000136560274 ) ) ;
#4517 = DIRECTION ( 'NONE',  ( -1.000000000000000000, 0.000000000000000000, -0.000000000000000000 ) ) ;
#4518 = CIRCLE ( 'NONE', #17914, 4.000000000000001776 ) ;
#4519 = AXIS2_PLACEMENT_3D ( 'NONE', #3753, #9413, #20392 ) ;
#4520 = FACE_OUTER_BOUND ( 'NONE', #17875, .T. ) ;
#4521 = ORIENTED_EDGE ( 'NONE', *, *, #16060, .F. ) ;
#4522 = CARTESIAN_POINT ( 'NONE',  ( 47.23681404676619877, -9.000000000000003553, 5.000000000000079936 ) ) ;
#4523 = MECHANICAL_DESIGN_GEOMETRIC_PRESENTATION_REPRESENTATION (  '', ( #18302 ), #19055 ) ;
#4524 = CARTESIAN_POINT ( 'NONE',  ( -1.656854249492380138, -3.999999999999999112, 12.18750000000001066 ) ) ;
#4525 = LINE ( 'NONE', #8142, #13128 ) ;
#4526 = VERTEX_POINT ( 'NONE', #4934 ) ;
#4527 = CARTESIAN_POINT ( 'NONE',  ( -1.594879469667249916, -11.25000000000000355, 10.00000000000008882 ) ) ;
#4528 = EDGE_CURVE ( 'NONE', #1949, #3403, #22264, .T. ) ;
#4529 = LINE ( 'NONE', #14000, #3704 ) ;
#4530 = PRODUCT_DEFINITION_CONTEXT ( 'detailed design', #21519, 'design' ) ;
#4531 = EDGE_CURVE ( 'NONE', #6311, #402, #1619, .T. ) ;
#4532 = CARTESIAN_POINT ( 'NONE',  ( 71.35000000218497007, 8.964466094067278235, 12.49999999999997691 ) ) ;
#4533 = ORIENTED_EDGE ( 'NONE', *, *, #14379, .F. ) ;
#4534 = CARTESIAN_POINT ( 'NONE',  ( -68.55000000218494449, 11.03553390593269157, 17.50000000000004619 ) ) ;
#4535 = ORIENTED_EDGE ( 'NONE', *, *, #13607, .T. ) ;
#4536 = DIRECTION ( 'NONE',  ( 0.000000000000000000, 0.000000000000000000, 1.000000000000000000 ) ) ;
#4537 =( BOUNDED_CURVE ( )  B_SPLINE_CURVE ( 2, ( #9111, #1536, #18306, #7189, #7316, #21768, #12718, #1888, #11146 ),
 .UNSPECIFIED., .F., .F. ) 
 B_SPLINE_CURVE_WITH_KNOTS ( ( 3, 2, 2, 2, 3 ),
 ( 0.6875000000000001110, 0.7031250000000000000, 0.7187500000000000000, 0.7343749999999998890, 0.7499999999999997780 ),
 .UNSPECIFIED. ) 
 CURVE ( )  GEOMETRIC_REPRESENTATION_ITEM ( )  RATIONAL_B_SPLINE_CURVE ( ( 0.9999999999999994449, 0.9238795325112872936, 1.000000000000000000, 0.9238795325112867385, 1.000000000000000000, 0.9238795325112867385, 1.000000000000000000, 0.9238795325112878487, 0.9999999999999988898 ) ) 
 REPRESENTATION_ITEM ( '' )  );
#4538 = CARTESIAN_POINT ( 'NONE',  ( -69.75000000218496155, 8.964466094067244484, 12.50000000000000711 ) ) ;
#4539 = EDGE_CURVE ( 'NONE', #17227, #22113, #4017, .T. ) ;
#4540 = CARTESIAN_POINT ( 'NONE',  ( 70.55000000218495870, 8.964466094067258695, 12.49999999999999289 ) ) ;
#4541 = EDGE_CURVE ( 'NONE', #7429, #5469, #8903, .T. ) ;
#4542 = CARTESIAN_POINT ( 'NONE',  ( 1.656854249492384135, -3.999999999999999112, 19.31250000000001421 ) ) ;
#4543 = TOROIDAL_SURFACE ( 'NONE', #23671, 8.800000000000022027, 0.2000000000000011768 ) ;
#4544 = CARTESIAN_POINT ( 'NONE',  ( -2.000000000000006661, 3.464101615137750834, 0.000000000000000000 ) ) ;
#4545 = CARTESIAN_POINT ( 'NONE',  ( 68.55000000109247082, 8.538419263543524096, 13.53841926354352054 ) ) ;
#4546 = ORIENTED_EDGE ( 'NONE', *, *, #16601, .T. ) ;
#4547 = CARTESIAN_POINT ( 'NONE',  ( -68.90000000218495302, 8.232233047033629347, 13.23223304703362402 ) ) ;
#4548 = LINE ( 'NONE', #17370, #2622 ) ;
#4549 = CARTESIAN_POINT ( 'NONE',  ( 69.70000000109246230, 12.06698730000000275, 15.85617417291294196 ) ) ;
#4550 = CARTESIAN_POINT ( 'NONE',  ( -2.445694354108819191, 2.445694354108820523, 15.31250000136560452 ) ) ;
#4551 = DIRECTION ( 'NONE',  ( -0.000000000000000000, -0.000000000000000000, 1.000000000000000000 ) ) ;
#4552 = VECTOR ( 'NONE', #8990, 1000.000000000000000 ) ;
#4553 = CARTESIAN_POINT ( 'NONE',  ( -14.99999999999997335, 15.00000000000000000, -49.99999999999999289 ) ) ;
#4554 = ORIENTED_EDGE ( 'NONE', *, *, #23267, .F. ) ;
#4555 = CARTESIAN_POINT ( 'NONE',  ( 4.000000000000000000, 1.656854249492381248, 0.8625000000000004885 ) ) ;
#4556 = CYLINDRICAL_SURFACE ( 'NONE', #14398, 4.000000000000001776 ) ;
#4557 = CARTESIAN_POINT ( 'NONE',  ( 2.499999999999999556, -7.958834565716711218, -7.593217523260672230 ) ) ;
#4558 = CARTESIAN_POINT ( 'NONE',  ( -2.828427124746190291, 2.828427124746190291, -0.8249999999999976241 ) ) ;
#4559 = PRODUCT_DEFINITION_SHAPE ( 'NONE', 'NONE',  #9760 ) ;
#4560 = ORIENTED_EDGE ( 'NONE', *, *, #9865, .F. ) ;
#4561 = ORIENTED_EDGE ( 'NONE', *, *, #7671, .T. ) ;
#4562 = CARTESIAN_POINT ( 'NONE',  ( -66.60000000109248219, 7.933012699999995476, 15.85617417291294196 ) ) ;
#4563 = ORIENTED_EDGE ( 'NONE', *, *, #8664, .T. ) ;
#4564 = CARTESIAN_POINT ( 'NONE',  ( -67.10000000109246798, 10.85617417291294551, 12.93301269999999370 ) ) ;
#4565 = CONTEXT_DEPENDENT_SHAPE_REPRESENTATION ( #7951, #22312 ) ;
#4566 = AXIS2_PLACEMENT_3D ( 'NONE', #10772, #16489, #18046 ) ;
#4567 = EDGE_CURVE ( 'NONE', #14572, #22615, #18079, .T. ) ;
#4568 = ORIENTED_EDGE ( 'NONE', *, *, #15106, .T. ) ;
#4569 = CARTESIAN_POINT ( 'NONE',  ( 22.11331769071655984, -8.974600000000002353, 5.000000000000079936 ) ) ;
#4570 = VERTEX_POINT ( 'NONE', #16433 ) ;
#4571 = EDGE_CURVE ( 'NONE', #17488, #2257, #10596, .T. ) ;
#4572 = ORIENTED_EDGE ( 'NONE', *, *, #23437, .T. ) ;
#4573 = CARTESIAN_POINT ( 'NONE',  ( 1.432654583217641386, 3.458734125000000770, 14.37500000136560452 ) ) ;
#4574 = CARTESIAN_POINT ( 'NONE',  ( 51.09375000000000000, 11.24264068711927322, 11.99999999999998934 ) ) ;
#4575 = ADVANCED_FACE ( 'NONE', ( #3368 ), #5408, .F. ) ;
#4576 = AXIS2_PLACEMENT_3D ( 'NONE', #11141, #18415, #5247 ) ;
#4577 = FACE_OUTER_BOUND ( 'NONE', #5978, .T. ) ;
#4578 = FACE_BOUND ( 'NONE', #10840, .T. ) ;
#4579 = CARTESIAN_POINT ( 'NONE',  ( -68.00000000109245946, 12.06698730000000275, 14.14382582708705094 ) ) ;
#4580 = CARTESIAN_POINT ( 'NONE',  ( -19.55556463033274284, -11.25000000000000355, 5.000000000000079936 ) ) ;
#4581 = CARTESIAN_POINT ( 'NONE',  ( 56.96643183416158251, 7.028187705514638672, 13.68930817193508531 ) ) ;
#4582 = DIRECTION ( 'NONE',  ( 0.000000000000000000, -3.469446951953615175E-16, -1.000000000000000000 ) ) ;
#4583 = CARTESIAN_POINT ( 'NONE',  ( 3.458734125000000770, 1.432654583217640498, 5.550000001365596347 ) ) ;
#4584 = CARTESIAN_POINT ( 'NONE',  ( 72.50000000000000000, 9.999999999999998224, 17.49999999999999645 ) ) ;
#4585 = CARTESIAN_POINT ( 'NONE',  ( 2.828427124746191179, 2.828427124746190291, 10.75000000273119660 ) ) ;
#4586 = CARTESIAN_POINT ( 'NONE',  ( 29.82104703033275328, -11.25000000000000355, 5.000000000000079936 ) ) ;
#4587 = AXIS2_PLACEMENT_3D ( 'NONE', #968, #20731, #2417 ) ;
#4588 = CIRCLE ( 'NONE', #22924, 4.000000000000000000 ) ;
#4589 = ORIENTED_EDGE ( 'NONE', *, *, #12262, .T. ) ;
#4590 = CARTESIAN_POINT ( 'NONE',  ( -1.656854249492379472, 4.000000000000000000, 16.93750000273119838 ) ) ;
#4591 = ORIENTED_EDGE ( 'NONE', *, *, #8075, .F. ) ;
#4592 = CARTESIAN_POINT ( 'NONE',  ( 52.65393183416158251, 6.971812294485357775, 16.17458954617365663 ) ) ;
#4593 = CARTESIAN_POINT ( 'NONE',  ( 3.458734125000000770, -1.432654583217639610, 2.175000001365597679 ) ) ;
#4594 = CARTESIAN_POINT ( 'NONE',  ( 1.125461230421587633, -3.270501301980698550, 2.040000000000001812 ) ) ;
#4595 = EDGE_LOOP ( 'NONE', ( #9732, #17463, #21178, #272 ) ) ;
#4596 = AXIS2_PLACEMENT_3D ( 'NONE', #15071, #9787, #10041 ) ;
#4597 = CARTESIAN_POINT ( 'NONE',  ( 47.24605889071655440, -8.974600000000002353, 10.00000000000008882 ) ) ;
#4598 = CARTESIAN_POINT ( 'NONE',  ( -20.00005079999999680, 5.400000000000000355, 1.000000000000000000 ) ) ;
#4599 = AXIS2_PLACEMENT_3D ( 'NONE', #3847, #21912, #16550 ) ;
#4600 = VERTEX_POINT ( 'NONE', #6975 ) ;
#4601 = DIRECTION ( 'NONE',  ( -1.000000000000000000, -0.000000000000000000, 0.000000000000000000 ) ) ;
#4602 = ORIENTED_EDGE ( 'NONE', *, *, #5326, .F. ) ;
#4603 = EDGE_CURVE ( 'NONE', #6374, #3871, #12508, .T. ) ;
#4604 = CARTESIAN_POINT ( 'NONE',  ( 58.72106816583844591, 13.02818770551464489, 16.17458954617363531 ) ) ;
#4605 = CARTESIAN_POINT ( 'NONE',  ( -71.45000000218495018, 11.03553390593273598, 12.49999999999999289 ) ) ;
#4606 = CARTESIAN_POINT ( 'NONE',  ( -71.80000000218494449, 9.999999999999998224, 17.49999999999999645 ) ) ;
#4607 = DIRECTION ( 'NONE',  ( 0.000000000000000000, 0.000000000000000000, 1.000000000000000000 ) ) ;
#4608 = CARTESIAN_POINT ( 'NONE',  ( -3.458734124999999437, 0.000000000000000000, 18.68750000136560629 ) ) ;
#4609 = CARTESIAN_POINT ( 'NONE',  ( 9.920644283265380691E-16, 4.000000000000000000, 11.87500000273119660 ) ) ;
#4610 = CARTESIAN_POINT ( 'NONE',  ( -20.00000000000001066, 1.500000000000003109, -50.00000000000000000 ) ) ;
#4611 = CIRCLE ( 'NONE', #18000, 8.073750000000021743 ) ;
#4612 = CARTESIAN_POINT ( 'NONE',  ( 70.35000000109248219, 11.46158073645647235, 16.46158073645647235 ) ) ;
#4613 = VECTOR ( 'NONE', #15, 1000.000000000000000 ) ;
#4614 = CARTESIAN_POINT ( 'NONE',  ( 10.15255810323380992, -9.000000000000001776, 10.00000000000008882 ) ) ;
#4615 = CARTESIAN_POINT ( 'NONE',  ( 52.43981816583844591, 10.06805114094563791, 17.99999999999999645 ) ) ;
#4616 = CARTESIAN_POINT ( 'NONE',  ( 1.432654583217642275, -3.458734124999999882, 3.300000001365598568 ) ) ;
#4617 = CARTESIAN_POINT ( 'NONE',  ( 3.458734125000002546, -1.432654583217639610, 11.12500000136560452 ) ) ;
#4618 = FACE_OUTER_BOUND ( 'NONE', #20979, .T. ) ;
#4619 = CARTESIAN_POINT ( 'NONE',  ( -68.50000000109245946, 7.933012699999995476, 14.14382582708705094 ) ) ;
#4620 = CARTESIAN_POINT ( 'NONE',  ( 4.999999999999999112, 0.000000000000000000, 0.000000000000000000 ) ) ;
#4621 = DIRECTION ( 'NONE',  ( -1.000000000000000000, -0.000000000000000000, -0.000000000000000000 ) ) ;
#4622 = ORIENTED_EDGE ( 'NONE', *, *, #9338, .T. ) ;
#4623 = LINE ( 'NONE', #11956, #4990 ) ;
#4624 = CARTESIAN_POINT ( 'NONE',  ( -2.828427124746190291, 2.828427124746190291, 3.300000002731189319 ) ) ;
#4625 = EDGE_LOOP ( 'NONE', ( #15397, #12308, #21653, #6134 ) ) ;
#4626 = VERTEX_POINT ( 'NONE', #5050 ) ;
#4627 = CARTESIAN_POINT ( 'NONE',  ( 34.36634005239895373, 10.78772952506732175, 10.00000000000008882 ) ) ;
#4628 = CARTESIAN_POINT ( 'NONE',  ( 51.75000000000000711, 7.171572875253819923, 17.82842712474619873 ) ) ;
#4629 = VERTEX_POINT ( 'NONE', #8660 ) ;
#4630 = DIRECTION ( 'NONE',  ( -7.087422195345011518E-32, -1.000000000000000000, -0.000000000000000000 ) ) ;
#4631 = AXIS2_PLACEMENT_3D ( 'NONE', #17620, #5379, #1537 ) ;
#4632 = CARTESIAN_POINT ( 'NONE',  ( 69.45000000109247651, 12.06698730000000097, 14.99999999999999645 ) ) ;
#4633 = CARTESIAN_POINT ( 'NONE',  ( 67.80000000109247082, 9.143825827087050939, 12.93301269999999370 ) ) ;
#4634 = VERTEX_POINT ( 'NONE', #3712 ) ;
#4635 = EDGE_CURVE ( 'NONE', #16065, #8909, #15960, .T. ) ;
#4636 = CARTESIAN_POINT ( 'NONE',  ( 4.999999999999999112, 0.000000000000000000, 0.000000000000000000 ) ) ;
#4637 = CARTESIAN_POINT ( 'NONE',  ( 58.87500000000000711, 7.171572875253794166, 12.17157287525381726 ) ) ;
#4638 = CARTESIAN_POINT ( 'NONE',  ( 71.60000000218494165, 12.50000000000000000, 14.99999999999999645 ) ) ;
#4639 = FACE_OUTER_BOUND ( 'NONE', #2126, .T. ) ;
#4640 = DIRECTION ( 'NONE',  ( 0.000000000000000000, 0.000000000000000000, 1.000000000000000000 ) ) ;
#4641 = DIRECTION ( 'NONE',  ( 0.000000000000000000, 0.8090169943749446757, 0.5877852522924770229 ) ) ;
#4642 = ORIENTED_EDGE ( 'NONE', *, *, #23438, .F. ) ;
#4643 = FACE_BOUND ( 'NONE', #15436, .T. ) ;
#4644 = CARTESIAN_POINT ( 'NONE',  ( 4.999999999999999112, 5.538577986808997267, -6.772677083992326708 ) ) ;
#4645 = CARTESIAN_POINT ( 'NONE',  ( 72.25000000109247367, 9.999999999999998224, 17.06698730000000097 ) ) ;
#4646 = EDGE_CURVE ( 'NONE', #4148, #872, #10827, .T. ) ;
#4647 = VERTEX_POINT ( 'NONE', #21554 ) ;
#4648 = CARTESIAN_POINT ( 'NONE',  ( 5.577176569667260608, -11.25000000000000355, 5.000000000000079936 ) ) ;
#4649 = DIRECTION ( 'NONE',  ( 1.000000000000000000, 0.000000000000000000, 0.000000000000000000 ) ) ;
#4650 = CARTESIAN_POINT ( 'NONE',  ( -65.00000000000000000, -15.00000000000000000, 20.00000000000001421 ) ) ;
#4651 = CARTESIAN_POINT ( 'NONE',  ( -2.247776618166720475, 3.308700692843488333, 9.970592379354943802 ) ) ;
#4652 = ORIENTED_EDGE ( 'NONE', *, *, #11929, .F. ) ;
#4653 = DIRECTION ( 'NONE',  ( -1.000000000000000000, -0.000000000000000000, -0.000000000000000000 ) ) ;
#4654 = ORIENTED_EDGE ( 'NONE', *, *, #23575, .F. ) ;
#4655 = CARTESIAN_POINT ( 'NONE',  ( 1.656854249492381470, 4.000000000000000000, 17.68750000000001066 ) ) ;
#4656 = CARTESIAN_POINT ( 'NONE',  ( 70.05000000218494449, 12.50000000000000000, 16.03553390593273420 ) ) ;
#4657 = CARTESIAN_POINT ( 'NONE',  ( 1.971781867644420635E-15, -4.000000000000000000, 16.25000000000001066 ) ) ;
#4658 = CARTESIAN_POINT ( 'NONE',  ( -14.99999999999997335, 15.00000000000000000, -49.99999999999999289 ) ) ;
#4659 = CARTESIAN_POINT ( 'NONE',  ( 68.65000000109246514, 9.999999999999998224, 12.93301269999999192 ) ) ;
#4660 = ORIENTED_EDGE ( 'NONE', *, *, #20365, .T. ) ;
#4661 = EDGE_CURVE ( 'NONE', #19572, #9951, #22893, .T. ) ;
#4662 = CARTESIAN_POINT ( 'NONE',  ( -68.65000000218495302, 8.964466094067214286, 17.49999999999996092 ) ) ;
#4663 = EDGE_CURVE ( 'NONE', #21869, #16726, #3939, .T. ) ;
#4664 = CARTESIAN_POINT ( 'NONE',  ( 1.656854249492384135, -3.999999999999999112, 10.43750000273119660 ) ) ;
#4665 = CARTESIAN_POINT ( 'NONE',  ( 70.10000000109245377, 7.933012699999995476, 14.14382582708705094 ) ) ;
#4666 = CARTESIAN_POINT ( 'NONE',  ( 3.458734125000002102, -1.432654583217639610, 12.87500000136560629 ) ) ;
#4667 = DIRECTION ( 'NONE',  ( -1.224646799147353207E-16, 0.000000000000000000, -1.000000000000000000 ) ) ;
#4668 = VERTEX_POINT ( 'NONE', #18341 ) ;
#4669 = CARTESIAN_POINT ( 'NONE',  ( 4.000000000000000000, 1.656854249492381248, -1.137499999999997513 ) ) ;
#4670 = CARTESIAN_POINT ( 'NONE',  ( -1.656854249492379472, 4.000000000000000000, 15.81250000000001066 ) ) ;
#4671 = DIRECTION ( 'NONE',  ( -1.000000000000000000, -0.000000000000000000, 0.000000000000000000 ) ) ;
#4672 = CARTESIAN_POINT ( 'NONE',  ( 4.000000000000000000, 4.898587196589412829E-16, -1.199999999999997957 ) ) ;
#4673 = ADVANCED_FACE ( 'NONE', ( #1441 ), #23371, .F. ) ;
#4674 = ADVANCED_FACE ( 'NONE', ( #1921 ), #7699, .T. ) ;
#4675 = ORIENTED_EDGE ( 'NONE', *, *, #22199, .F. ) ;
#4676 = DIRECTION ( 'NONE',  ( -1.000000000000000000, -6.123233995736827666E-17, 0.000000000000000000 ) ) ;
#4677 = ORIENTED_EDGE ( 'NONE', *, *, #17117, .F. ) ;
#4678 = CARTESIAN_POINT ( 'NONE',  ( -66.40000000109247935, 12.06698730000000275, 14.14382582708705094 ) ) ;
#4679 =( BOUNDED_CURVE ( )  B_SPLINE_CURVE ( 2, ( #11473, #15179, #22073, #22201, #13383, #20651, #3888, #11108, #9778 ),
 .UNSPECIFIED., .F., .F. ) 
 B_SPLINE_CURVE_WITH_KNOTS ( ( 3, 2, 2, 2, 3 ),
 ( 0.8124999999999993339, 0.8281249999999992228, 0.8437499999999991118, 0.8593749999999991118, 0.8749999999999990008 ),
 .UNSPECIFIED. ) 
 CURVE ( )  GEOMETRIC_REPRESENTATION_ITEM ( )  RATIONAL_B_SPLINE_CURVE ( ( 1.000000000000003331, 0.9238795325112835188, 1.000000000000000000, 0.9238795325112867385, 1.000000000000000000, 0.9238795325112867385, 1.000000000000000000, 0.9238795325112916235, 0.9999999999999951150 ) ) 
 REPRESENTATION_ITEM ( '' )  );
#4680 = VERTEX_POINT ( 'NONE', #18454 ) ;
#4681 = CARTESIAN_POINT ( 'NONE',  ( -90.00000000000000000, 1.012170579495290078E-15, 8.265000000000021885 ) ) ;
#4682 = ORIENTED_EDGE ( 'NONE', *, *, #21627, .T. ) ;
#4683 = ORIENTED_EDGE ( 'NONE', *, *, #6472, .F. ) ;
#4684 = CARTESIAN_POINT ( 'NONE',  ( -1.432654583217639832, -3.458734125000000326, 13.87500000136560452 ) ) ;
#4685 = LINE ( 'NONE', #15842, #9610 ) ;
#4686 = LINE ( 'NONE', #15737, #13296 ) ;
#4687 = EDGE_CURVE ( 'NONE', #19427, #19833, #2399, .T. ) ;
#4688 = CARTESIAN_POINT ( 'NONE',  ( 66.45000000109247651, 9.999999999999998224, 17.06698730000000097 ) ) ;
#4689 = VECTOR ( 'NONE', #23241, 1000.000000000000000 ) ;
#4690 = CARTESIAN_POINT ( 'NONE',  ( -69.89999999999999147, 12.50000000000000000, 14.99999999999999645 ) ) ;
#4691 = B_SPLINE_CURVE_WITH_KNOTS ( 'NONE', 3,
 ( #22847, #15583, #18904, #6460, #2379, #10071, #15461, #17361 ),
 .UNSPECIFIED., .F., .F.,
 ( 4, 2, 2, 4 ),
 ( 0.003797433802554448044, 0.004743183970586243095, 0.005688934138618039447, 0.007580434474681627816 ),
 .UNSPECIFIED. ) ;
#4692 = EDGE_CURVE ( 'NONE', #2020, #1924, #14285, .T. ) ;
#4693 = CARTESIAN_POINT ( 'NONE',  ( -4.000000000000000000, 0.000000000000000000, 0.4250000027311868211 ) ) ;
#4694 = CARTESIAN_POINT ( 'NONE',  ( 60.15393183416158962, 5.971812294485358663, 16.58880310854675599 ) ) ;
#4695 = DIRECTION ( 'NONE',  ( 0.000000000000000000, 1.000000000000000000, 0.000000000000000000 ) ) ;
#4696 = CARTESIAN_POINT ( 'NONE',  ( -1.432654583217641164, -3.458734125000000326, 1.175000001365597013 ) ) ;
#4697 = CARTESIAN_POINT ( 'NONE',  ( 67.30000000218494449, 8.232233047033629347, 13.23223304703362402 ) ) ;
#4698 = CARTESIAN_POINT ( 'NONE',  ( 71.64999999999997726, 11.03553390593269867, 17.50000000000003908 ) ) ;
#4699 = CARTESIAN_POINT ( 'NONE',  ( -3.999999999999999112, 1.656854249492380804, 12.06250000273119838 ) ) ;
#4700 = DIRECTION ( 'NONE',  ( 0.9413949561959078505, 0.3373062947069098150, 0.000000000000000000 ) ) ;
#4701 = ADVANCED_FACE ( 'NONE', ( #16548 ), #11656, .F. ) ;
#4702 = EDGE_CURVE ( 'NONE', #19814, #21750, #7004, .T. ) ;
#4703 = ORIENTED_EDGE ( 'NONE', *, *, #10465, .T. ) ;
#4704 = DIRECTION ( 'NONE',  ( 1.000000000000000000, -0.000000000000000000, -0.000000000000000000 ) ) ;
#4705 = EDGE_LOOP ( 'NONE', ( #2637, #14161, #6964, #16870 ) ) ;
#4706 = CARTESIAN_POINT ( 'NONE',  ( 52.37268183416157541, 7.926799079670491466, 12.83056023321021755 ) ) ;
#4707 = PRESENTATION_STYLE_ASSIGNMENT (( #19303 ) ) ;
#4708 = CARTESIAN_POINT ( 'NONE',  ( 2.445694354108820079, 2.445694354108820523, 1.362500001365595903 ) ) ;
#4709 = EDGE_LOOP ( 'NONE', ( #13314, #3189, #12036, #8234 ) ) ;
#4710 = CARTESIAN_POINT ( 'NONE',  ( -65.00000000000000000, 9.999999999999998224, 25.00000000000001421 ) ) ;
#4711 = CIRCLE ( 'NONE', #13910, 2.649999999999992806 ) ;
#4712 = AXIS2_PLACEMENT_3D ( 'NONE', #15481, #1066, #15244 ) ;
#4713 = ORIENTED_EDGE ( 'NONE', *, *, #2592, .T. ) ;
#4714 = LINE ( 'NONE', #6869, #20578 ) ;
#4715 = VERTEX_POINT ( 'NONE', #5768 ) ;
#4716 = CARTESIAN_POINT ( 'NONE',  ( 57.87731816583843170, 7.830560233210212218, 12.92679907967049679 ) ) ;
#4717 = CARTESIAN_POINT ( 'NONE',  ( -68.80000000218494449, 7.499999999999996447, 14.99999999999999645 ) ) ;
#4718 = CARTESIAN_POINT ( 'NONE',  ( -0.3649867057748917842, 3.983313282257320509, 9.889028792932920808 ) ) ;
#4719 = FACE_OUTER_BOUND ( 'NONE', #15486, .T. ) ;
#4720 = CARTESIAN_POINT ( 'NONE',  ( 1.872352939448454495E-15, -3.458734125000000770, 18.93750000136560629 ) ) ;
#4721 = CARTESIAN_POINT ( 'NONE',  ( 1.971781867644420635E-15, -4.000000000000000000, 14.37500000273119660 ) ) ;
#4722 = CARTESIAN_POINT ( 'NONE',  ( 58.59375000000000711, 11.24264068711927322, 11.99999999999998934 ) ) ;
#4723 = CARTESIAN_POINT ( 'NONE',  ( 68.90000000109247935, 9.143825827087049163, 17.06698729999999742 ) ) ;
#4724 = VECTOR ( 'NONE', #21885, 1000.000000000000000 ) ;
#4725 = CARTESIAN_POINT ( 'NONE',  ( -4.204015924366189871, 1.626724848190922446, -3.610627190413390419 ) ) ;
#4726 = CARTESIAN_POINT ( 'NONE',  ( 57.87731816583843170, 7.830560233210212218, 12.92679907967049679 ) ) ;
#4727 = AXIS2_PLACEMENT_3D ( 'NONE', #12245, #19513, #3110 ) ;
#4728 = CARTESIAN_POINT ( 'NONE',  ( 1.432654583217640276, 3.458734125000000770, 2.675000001365597679 ) ) ;
#4729 = CARTESIAN_POINT ( 'NONE',  ( 1.872352939448454495E-15, -3.458734125000000770, 10.93750000136560452 ) ) ;
#4730 = EDGE_CURVE ( 'NONE', #13130, #3140, #4852, .T. ) ;
#4731 = CARTESIAN_POINT ( 'NONE',  ( 0.000000000000000000, 7.958834565716877307, -7.593217523260497259 ) ) ;
#4732 = CARTESIAN_POINT ( 'NONE',  ( -68.30000000109247082, 9.143825827087049163, 17.06698730000000097 ) ) ;
#4733 = EDGE_CURVE ( 'NONE', #13757, #2729, #15243, .T. ) ;
#4734 = ORIENTED_EDGE ( 'NONE', *, *, #19346, .T. ) ;
#4735 = CARTESIAN_POINT ( 'NONE',  ( 4.000000000000000000, -2.309401076758514915, -3.433295621305383349 ) ) ;
#4736 = CARTESIAN_POINT ( 'NONE',  ( 65.65000000218495302, 7.499999999999996447, 13.96446609406725514 ) ) ;
#4737 = ORIENTED_EDGE ( 'NONE', *, *, #3105, .T. ) ;
#4738 = CARTESIAN_POINT ( 'NONE',  ( 25.86052135323381407, -9.000000000000001776, 10.00000000000008882 ) ) ;
#4739 = CARTESIAN_POINT ( 'NONE',  ( -2.828427124746189403, -2.828427124746190735, 2.550000002731188875 ) ) ;
#4740 = ORIENTED_EDGE ( 'NONE', *, *, #11011, .T. ) ;
#4741 = ORIENTED_EDGE ( 'NONE', *, *, #14745, .T. ) ;
#4742 = CARTESIAN_POINT ( 'NONE',  ( -1.828356344711647319, -3.563200125723192002, -1.076197711133951296E-14 ) ) ;
#4743 = DIRECTION ( 'NONE',  ( 0.000000000000000000, 0.000000000000000000, -1.000000000000000000 ) ) ;
#4744 = ORIENTED_EDGE ( 'NONE', *, *, #8502, .T. ) ;
#4745 = UNCERTAINTY_MEASURE_WITH_UNIT (LENGTH_MEASURE( 1.000000000000000082E-05 ), #17997, 'distance_accuracy_value', 'NONE');
#4746 = CARTESIAN_POINT ( 'NONE',  ( 66.85000000109248219, 9.999999999999998224, 12.93301269999999192 ) ) ;
#4747 = CARTESIAN_POINT ( 'NONE',  ( 67.60000000109246798, 7.933012699999995476, 15.85617417291294196 ) ) ;
#4748 = DIRECTION ( 'NONE',  ( -0.000000000000000000, -0.000000000000000000, 1.000000000000000000 ) ) ;
#4749 = DIRECTION ( 'NONE',  ( 1.000000000000000000, 0.000000000000000000, 0.000000000000000000 ) ) ;
#4750 = CARTESIAN_POINT ( 'NONE',  ( 53.34375000000000000, 8.343145750507638070, 19.00000000000000711 ) ) ;
#4751 = CARTESIAN_POINT ( 'NONE',  ( -2.117863837641485618E-16, 3.458734125000000326, 2.487500001365596791 ) ) ;
#4752 = CARTESIAN_POINT ( 'NONE',  ( 3.458734125000002102, -1.432654583217639610, 13.87500000136560452 ) ) ;
#4753 = CARTESIAN_POINT ( 'NONE',  ( 68.05000000218494449, 7.499999999999996447, 13.96446609406725514 ) ) ;
#4754 = DIRECTION ( 'NONE',  ( -1.000000000000000000, -7.703719777548943412E-32, 0.000000000000000000 ) ) ;
#4755 = ORIENTED_EDGE ( 'NONE', *, *, #8201, .F. ) ;
#4756 = FACE_OUTER_BOUND ( 'NONE', #5320, .T. ) ;
#4757 = DIRECTION ( 'NONE',  ( 0.000000000000000000, 0.000000000000000000, 1.000000000000000000 ) ) ;
#4758 = LINE ( 'NONE', #21503, #22262 ) ;
#4759 = B_SPLINE_CURVE_WITH_KNOTS ( 'NONE', 3,
 ( #6349, #10318, #19498, #1171, #13663, #15923, #20924, #4544 ),
 .UNSPECIFIED., .F., .F.,
 ( 4, 2, 2, 4 ),
 ( 2.465131517071352357E-07, 0.001183067374689843057, 0.001774477805458910071, 0.002365888236227977302 ),
 .UNSPECIFIED. ) ;
#4760 = VERTEX_POINT ( 'NONE', #9373 ) ;
#4761 = CARTESIAN_POINT ( 'NONE',  ( 3.511755186886750923, -2.826662030176382956, -3.597382984111582083 ) ) ;
#4762 = CARTESIAN_POINT ( 'NONE',  ( 71.85000000109246798, 12.06698730000000097, 14.99999999999999645 ) ) ;
#4763 = CARTESIAN_POINT ( 'NONE',  ( 71.05000000218497291, 8.964466094067221391, 17.49999999999996447 ) ) ;
#4764 = VERTEX_POINT ( 'NONE', #16663 ) ;
#4765 = DIRECTION ( 'NONE',  ( -0.000000000000000000, -0.000000000000000000, 1.000000000000000000 ) ) ;
#4766 = ORIENTED_EDGE ( 'NONE', *, *, #20431, .T. ) ;
#4767 = EDGE_CURVE ( 'NONE', #7292, #20172, #8865, .T. ) ;
#4768 = DIRECTION ( 'NONE',  ( 0.000000000000000000, 0.000000000000000000, 1.000000000000000000 ) ) ;
#4769 = CIRCLE ( 'NONE', #11692, 4.000000000000000888 ) ;
#4770 = CONICAL_SURFACE ( 'NONE', #21190, 6.500000000000000888, 1.047197551196596521 ) ;
#4771 = CARTESIAN_POINT ( 'NONE',  ( 70.35000000218492744, 7.499999999999995559, 16.03553390593273420 ) ) ;
#4772 = CARTESIAN_POINT ( 'NONE',  ( -3.803704290982251823, 5.309483803148794756, 4.394406930355310159E-15 ) ) ;
#4773 = CARTESIAN_POINT ( 'NONE',  ( 0.000000000000000000, 5.051668046482832750E-16, -4.000000000000000000 ) ) ;
#4774 = CARTESIAN_POINT ( 'NONE',  ( 67.35000000109246798, 11.46158073645647235, 16.46158073645647235 ) ) ;
#4775 = ORIENTED_EDGE ( 'NONE', *, *, #8623, .T. ) ;
#4776 = DIRECTION ( 'NONE',  ( 0.000000000000000000, 0.5877852522924743583, -0.8090169943749466741 ) ) ;
#4777 = CARTESIAN_POINT ( 'NONE',  ( 70.75000000109247367, 8.538419263543522320, 16.46158073645647235 ) ) ;
#4778 = CARTESIAN_POINT ( 'NONE',  ( -1.432654583217639610, -3.458734124999999882, 10.62500000136560274 ) ) ;
#4779 = DIRECTION ( 'NONE',  ( -0.000000000000000000, -0.000000000000000000, 1.000000000000000000 ) ) ;
#4780 = CIRCLE ( 'NONE', #4411, 4.000000000000000000 ) ;
#4781 = CARTESIAN_POINT ( 'NONE',  ( 6.500000000000000000, 3.752776749732573247, -0.5805565836007695601 ) ) ;
#4782 = ORIENTED_EDGE ( 'NONE', *, *, #1455, .F. ) ;
#4783 = CARTESIAN_POINT ( 'NONE',  ( 1.656854249492383024, -3.999999999999999112, -2.387499999999998401 ) ) ;
#4784 = CARTESIAN_POINT ( 'NONE',  ( 60.00000000000000711, 9.999999999999998224, 24.99999999999999645 ) ) ;
#4785 = AXIS2_PLACEMENT_3D ( 'NONE', #14114, #15905, #8368 ) ;
#4786 = FACE_OUTER_BOUND ( 'NONE', #1805, .T. ) ;
#4787 = DIRECTION ( 'NONE',  ( 0.000000000000000000, 0.9510565162951523099, 0.3090169943749515591 ) ) ;
#4788 = ORIENTED_EDGE ( 'NONE', *, *, #13087, .T. ) ;
#4789 = LINE ( 'NONE', #1298, #23520 ) ;
#4790 = ORIENTED_EDGE ( 'NONE', *, *, #7529, .T. ) ;
#4791 = CARTESIAN_POINT ( 'NONE',  ( -68.35000000109246798, 8.538419263543522320, 16.46158073645647235 ) ) ;
#4792 = CONTEXT_DEPENDENT_SHAPE_REPRESENTATION ( #19396, #18883 ) ;
#4793 = ORIENTED_EDGE ( 'NONE', *, *, #13206, .T. ) ;
#4794 = CARTESIAN_POINT ( 'NONE',  ( -66.10000000218495586, 11.76776695296636888, 16.76776695296636532 ) ) ;
#4795 = ORIENTED_EDGE ( 'NONE', *, *, #4571, .T. ) ;
#4796 = EDGE_CURVE ( 'NONE', #16763, #12570, #487, .T. ) ;
#4797 = EDGE_CURVE ( 'NONE', #5511, #5170, #13325, .T. ) ;
#4798 = ORIENTED_EDGE ( 'NONE', *, *, #22573, .T. ) ;
#4799 = CARTESIAN_POINT ( 'NONE',  ( 1.432654583217641386, 3.458734125000000770, 12.37500000136560629 ) ) ;
#4800 = CARTESIAN_POINT ( 'NONE',  ( 0.000000000000000000, 0.000000000000000000, -5.000000000000000000 ) ) ;
#4801 = VECTOR ( 'NONE', #21071, 999.9999999999997726 ) ;
#4802 = CARTESIAN_POINT ( 'NONE',  ( -68.05000000218494449, 7.499999999999996447, 13.96446609406725514 ) ) ;
#4803 = LINE ( 'NONE', #10107, #13346 ) ;
#4804 = EDGE_CURVE ( 'NONE', #18480, #22910, #11543, .T. ) ;
#4805 = CARTESIAN_POINT ( 'NONE',  ( -69.54999999999999716, 7.499999999999995559, 13.96446609406725692 ) ) ;
#4806 = CARTESIAN_POINT ( 'NONE',  ( -71.64999999999997726, 11.03553390593269867, 17.50000000000003908 ) ) ;
#4807 = CARTESIAN_POINT ( 'NONE',  ( 59.99999999999995026, 12.78483204250637328, 17.66020603153145885 ) ) ;
#4808 = AXIS2_PLACEMENT_3D ( 'NONE', #6362, #22750, #13677 ) ;
#4809 =( BOUNDED_CURVE ( )  B_SPLINE_CURVE ( 2, ( #14809, #18606, #20511, #11455, #1955 ),
 .UNSPECIFIED., .F., .F. ) 
 B_SPLINE_CURVE_WITH_KNOTS ( ( 3, 2, 3 ),
 ( 0.4260621439306495062, 0.4375000000000000000, 0.4500000000000000111 ),
 .UNSPECIFIED. ) 
 CURVE ( )  GEOMETRIC_REPRESENTATION_ITEM ( )  RATIONAL_B_SPLINE_CURVE ( ( 0.9881630608388305426, 0.9303476039145940346, 1.000000000000000000, 0.9238795325112867385, 1.000000000000000000 ) ) 
 REPRESENTATION_ITEM ( '' )  );
#4810 = CARTESIAN_POINT ( 'NONE',  ( 2.445694354108820967, -2.445694354108820079, -1.637499998634403209 ) ) ;
#4811 = CARTESIAN_POINT ( 'NONE',  ( -3.999999999999999112, 0.000000000000000000, 13.00000000000001066 ) ) ;
#4812 = FACE_OUTER_BOUND ( 'NONE', #4150, .T. ) ;
#4813 = CARTESIAN_POINT ( 'NONE',  ( -2.828427124746188515, -2.828427124746190735, 13.25000000273119660 ) ) ;
#4814 = CARTESIAN_POINT ( 'NONE',  ( 0.000000000000000000, 4.714285714285714413, 3.059999999999998277 ) ) ;
#4815 = ORIENTED_EDGE ( 'NONE', *, *, #20190, .F. ) ;
#4816 = CARTESIAN_POINT ( 'NONE',  ( -71.25000000109248788, 9.999999999999998224, 17.06698730000000097 ) ) ;
#4817 = ORIENTED_EDGE ( 'NONE', *, *, #16677, .F. ) ;
#4818 = CARTESIAN_POINT ( 'NONE',  ( 53.40393183416157541, 13.02818770551463778, 13.82541045382633982 ) ) ;
#4819 = CARTESIAN_POINT ( 'NONE',  ( -69.30000000109247082, 10.85617417291294551, 12.93301269999999370 ) ) ;
#4820 = SURFACE_SIDE_STYLE ('',( #20972 ) ) ;
#4821 = CARTESIAN_POINT ( 'NONE',  ( 3.458734125000001214, -1.432654583217639610, 1.175000001365597013 ) ) ;
#4822 = VERTEX_POINT ( 'NONE', #4784 ) ;
#4823 = CARTESIAN_POINT ( 'NONE',  ( 6.500000000000000000, 3.752776749732573247, -0.5805565836007695601 ) ) ;
#4824 = EDGE_CURVE ( 'NONE', #8665, #1978, #21149, .T. ) ;
#4825 = EDGE_LOOP ( 'NONE', ( #10672, #20703, #8293, #4112 ) ) ;
#4826 = CARTESIAN_POINT ( 'NONE',  ( 2.500000000000000000, 2.357898499370431722, -2.818925648462311528E-15 ) ) ;
#4827 = ORIENTED_EDGE ( 'NONE', *, *, #21792, .T. ) ;
#4828 = CARTESIAN_POINT ( 'NONE',  ( 57.22106816583844591, 13.02818770551464489, 16.17458954617363531 ) ) ;
#4829 = CARTESIAN_POINT ( 'NONE',  ( -66.10000000218495586, 11.76776695296636888, 16.76776695296636532 ) ) ;
#4830 = EDGE_CURVE ( 'NONE', #2790, #12003, #13804, .T. ) ;
#4831 = CARTESIAN_POINT ( 'NONE',  ( 21.00000000000000000, 2.055000000000000160, 0.000000000000000000 ) ) ;
#4832 = EDGE_CURVE ( 'NONE', #3912, #7937, #21240, .T. ) ;
#4833 = CARTESIAN_POINT ( 'NONE',  ( -71.70000000109247651, 7.933012699999995476, 14.14382582708705094 ) ) ;
#4834 = CARTESIAN_POINT ( 'NONE',  ( -2.445694354108819191, 2.445694354108820523, 16.56250000136560629 ) ) ;
#4835 = CARTESIAN_POINT ( 'NONE',  ( 1.656854249492381470, 4.000000000000000000, 12.81250000273119660 ) ) ;
#4836 = CARTESIAN_POINT ( 'NONE',  ( 59.81250000000000711, 13.00000000000000000, 14.99999999999998757 ) ) ;
#4837 = CARTESIAN_POINT ( 'NONE',  ( 68.20000000109246230, 7.933012699999995476, 15.85617417291294196 ) ) ;
#4838 = CARTESIAN_POINT ( 'NONE',  ( 0.000000000000000000, 9.314797388894893615, 1.239665997526919083 ) ) ;
#4839 = CARTESIAN_POINT ( 'NONE',  ( 51.40856816583843880, 12.97181229448534978, 13.68930817193506755 ) ) ;
#4840 = CARTESIAN_POINT ( 'NONE',  ( 1.432654583217640276, 3.458734125000000770, -0.3249999986344045411 ) ) ;
#4841 = CARTESIAN_POINT ( 'NONE',  ( 67.55000000218494449, 12.50000000000000000, 13.96446609406725692 ) ) ;
#4842 = LINE ( 'NONE', #15657, #13015 ) ;
#4843 = CARTESIAN_POINT ( 'NONE',  ( -67.95000000109247651, 11.46158073645647235, 13.53841926354352232 ) ) ;
#4844 = VERTEX_POINT ( 'NONE', #15600 ) ;
#4845 = DIRECTION ( 'NONE',  ( 0.000000000000000000, 0.000000000000000000, -1.000000000000000000 ) ) ;
#4846 = DIRECTION ( 'NONE',  ( -1.000000000000000000, 0.000000000000000000, 0.000000000000000000 ) ) ;
#4847 = VERTEX_POINT ( 'NONE', #20828 ) ;
#4848 = CARTESIAN_POINT ( 'NONE',  ( -3.999999999999999112, 0.000000000000000000, 15.12500000273119660 ) ) ;
#4849 = CARTESIAN_POINT ( 'NONE',  ( -2.828427124746190291, 2.828427124746190291, 0.3000000027311867101 ) ) ;
#4850 = ORIENTED_EDGE ( 'NONE', *, *, #13903, .T. ) ;
#4851 = ORIENTED_EDGE ( 'NONE', *, *, #13083, .F. ) ;
#4852 =( BOUNDED_CURVE ( )  B_SPLINE_CURVE ( 2, ( #124, #598, #7924, #7455, #9485, #5998, #16785, #2281, #14770 ),
 .UNSPECIFIED., .F., .F. ) 
 B_SPLINE_CURVE_WITH_KNOTS ( ( 3, 2, 2, 2, 3 ),
 ( 0.6999999999999999556, 0.7125000000000000222, 0.7249999999999999778, 0.7375000000000000444, 0.7500000000000000000 ),
 .UNSPECIFIED. ) 
 CURVE ( )  GEOMETRIC_REPRESENTATION_ITEM ( )  RATIONAL_B_SPLINE_CURVE ( ( 1.000000000000000000, 0.9238795325112867385, 1.000000000000000000, 0.9238795325112867385, 1.000000000000000000, 0.9238795325112867385, 1.000000000000000000, 0.9238795325112867385, 1.000000000000000000 ) ) 
 REPRESENTATION_ITEM ( '' )  );
#4853 = FACE_BOUND ( 'NONE', #16948, .T. ) ;
#4854 = VECTOR ( 'NONE', #3628, 1000.000000000000000 ) ;
#4855 = EDGE_CURVE ( 'NONE', #19246, #14210, #15827, .T. ) ;
#4856 = CARTESIAN_POINT ( 'NONE',  ( 2.100000000000000089, 0.000000000000000000, -5.000000000000000000 ) ) ;
#4857 = ORIENTED_EDGE ( 'NONE', *, *, #12635, .T. ) ;
#4858 = CARTESIAN_POINT ( 'NONE',  ( 2.836893136758676270, 3.208949435745843903, -3.505054077164911241 ) ) ;
#4859 = APPLICATION_CONTEXT ( 'automotive_design' ) ;
#4860 = EDGE_CURVE ( 'NONE', #1132, #17303, #16196, .T. ) ;
#4861 = CARTESIAN_POINT ( 'NONE',  ( 65.95000000109247651, 8.538419263543524096, 13.53841926354352054 ) ) ;
#4862 = CIRCLE ( 'NONE', #18300, 8.749000000000002331 ) ;
#4863 = VECTOR ( 'NONE', #12869, 1000.000000000000000 ) ;
#4864 = EDGE_CURVE ( 'NONE', #18254, #19389, #22868, .T. ) ;
#4865 = CARTESIAN_POINT ( 'NONE',  ( 68.05000000109247082, 12.06698730000000097, 14.99999999999999645 ) ) ;
#4866 = CARTESIAN_POINT ( 'NONE',  ( -60.00000000000000711, -15.00000000000000000, 10.00000000000008882 ) ) ;
#4867 = DIRECTION ( 'NONE',  ( 0.000000000000000000, -1.287488025362403787E-15, -1.000000000000000000 ) ) ;
#4868 = CARTESIAN_POINT ( 'NONE',  ( 58.43981816583843170, 10.06805114094564857, 19.00000000000000000 ) ) ;
#4869 = CARTESIAN_POINT ( 'NONE',  ( -3.458734125000000326, 1.432654583217640276, 2.675000001365597679 ) ) ;
#4870 = CARTESIAN_POINT ( 'NONE',  ( 2.445694354108821855, -2.445694354108820079, 13.81250000136560629 ) ) ;
#4871 = FACE_OUTER_BOUND ( 'NONE', #9488, .T. ) ;
#4872 = VECTOR ( 'NONE', #13723, 1000.000000000000000 ) ;
#4873 = CARTESIAN_POINT ( 'NONE',  ( 118.3095189484530181, -10.00000000000001954, 15.00000000000002842 ) ) ;
#4874 = ORIENTED_EDGE ( 'NONE', *, *, #18393, .F. ) ;
#4875 = DIRECTION ( 'NONE',  ( -1.000000000000000000, 0.000000000000000000, -0.000000000000000000 ) ) ;
#4876 = CARTESIAN_POINT ( 'NONE',  ( 68.09999999999999432, 9.999999999999998224, 12.49999999999999289 ) ) ;
#4877 = CARTESIAN_POINT ( 'NONE',  ( 0.000000000000000000, 0.000000000000000000, 5.000000000000008882 ) ) ;
#4878 = AXIS2_PLACEMENT_3D ( 'NONE', #20060, #5589, #20180 ) ;
#4879 = VECTOR ( 'NONE', #576, 1000.000000000000114 ) ;
#4880 = ORIENTED_EDGE ( 'NONE', *, *, #12990, .T. ) ;
#4881 = CARTESIAN_POINT ( 'NONE',  ( 45.52901028033275566, -11.25000000000000355, 5.000000000000079936 ) ) ;
#4882 = CARTESIAN_POINT ( 'NONE',  ( -67.54999999999999716, 12.50000000000000000, 16.03553390593273775 ) ) ;
#4883 = DIRECTION ( 'NONE',  ( 1.000000000000000000, -0.000000000000000000, -0.000000000000000000 ) ) ;
#4884 = ORIENTED_EDGE ( 'NONE', *, *, #21029, .T. ) ;
#4885 = CARTESIAN_POINT ( 'NONE',  ( -68.35000000218495586, 12.50000000000000000, 13.96446609406725692 ) ) ;
#4886 = ORIENTED_EDGE ( 'NONE', *, *, #7529, .F. ) ;
#4887 = CARTESIAN_POINT ( 'NONE',  ( 51.09375000000000000, 11.65685424949236193, 10.99999999999998401 ) ) ;
#4888 = VECTOR ( 'NONE', #6882, 1000.000000000000000 ) ;
#4889 = EDGE_CURVE ( 'NONE', #22418, #8553, #17142, .T. ) ;
#4890 = ADVANCED_FACE ( 'NONE', ( #15368 ), #4556, .T. ) ;
#4891 = CARTESIAN_POINT ( 'NONE',  ( 69.70000000218495018, 8.232233047033629347, 13.23223304703362402 ) ) ;
#4892 = VECTOR ( 'NONE', #15943, 1000.000000000000000 ) ;
#4893 = CARTESIAN_POINT ( 'NONE',  ( 6.500000000000000000, 3.145973671264227889, -3.294612376748629057 ) ) ;
#4894 = DIRECTION ( 'NONE',  ( -1.000000000000000000, 0.000000000000000000, 0.000000000000000000 ) ) ;
#4895 = CARTESIAN_POINT ( 'NONE',  ( 66.50000000109245946, 12.06698729999999919, 15.85617417291294196 ) ) ;
#4896 = ORIENTED_EDGE ( 'NONE', *, *, #12326, .F. ) ;
#4897 = CIRCLE ( 'NONE', #17155, 4.000000000000002665 ) ;
#4898 = AXIS2_PLACEMENT_3D ( 'NONE', #2786, #15520, #8204 ) ;
#4899 = DIRECTION ( 'NONE',  ( -1.000000000000000000, 0.000000000000000000, 1.445602896647339163E-16 ) ) ;
#4900 = CARTESIAN_POINT ( 'NONE',  ( -4.000000000000000000, 0.000000000000000000, -1.574999997268811569 ) ) ;
#4901 = CARTESIAN_POINT ( 'NONE',  ( 68.30000000109247082, 9.143825827087049163, 17.06698729999999742 ) ) ;
#4902 = CARTESIAN_POINT ( 'NONE',  ( -3.458734124999999437, 1.432654583217640498, 18.62500000136560274 ) ) ;
#4903 = CARTESIAN_POINT ( 'NONE',  ( -72.05000000109247082, 9.999999999999998224, 17.06698730000000097 ) ) ;
#4904 = TOROIDAL_SURFACE ( 'NONE', #15262, 5.384454397937118664, 0.5155456020628804703 ) ;
#4905 = CARTESIAN_POINT ( 'NONE',  ( 0.000000000000000000, 0.000000000000000000, 2.039999999999998259 ) ) ;
#4906 = ORIENTED_EDGE ( 'NONE', *, *, #12223, .T. ) ;
#4907 = CARTESIAN_POINT ( 'NONE',  ( -19.99999999999999645, -15.00000000000001954, 5.000000000000079936 ) ) ;
#4908 = CARTESIAN_POINT ( 'NONE',  ( -11.84783529071655295, -8.974600000000002353, 5.000000000000079936 ) ) ;
#4909 = CARTESIAN_POINT ( 'NONE',  ( 9.537702246766203373, -9.000000000000003553, 5.000000000000079936 ) ) ;
#4910 = ORIENTED_EDGE ( 'NONE', *, *, #22388, .T. ) ;
#4911 = CONICAL_SURFACE ( 'NONE', #7987, 4.000000000000000000, 0.8911886515913786111 ) ;
#4912 = CARTESIAN_POINT ( 'NONE',  ( -3.999999999999999112, 0.000000000000000000, 13.12500000273119660 ) ) ;
#4913 = ORIENTED_EDGE ( 'NONE', *, *, #8339, .T. ) ;
#4914 = LINE ( 'NONE', #10691, #5536 ) ;
#4915 = VERTEX_POINT ( 'NONE', #13559 ) ;
#4916 = DIRECTION ( 'NONE',  ( -1.000000000000000000, 0.000000000000000000, 1.224646799147353207E-16 ) ) ;
#4917 = ORIENTED_EDGE ( 'NONE', *, *, #4364, .T. ) ;
#4918 = VECTOR ( 'NONE', #8120, 1000.000000000000114 ) ;
#4919 = ORIENTED_EDGE ( 'NONE', *, *, #4687, .F. ) ;
#4920 = CARTESIAN_POINT ( 'NONE',  ( -1.432654583217639166, 3.458734125000000770, 12.50000000136560452 ) ) ;
#4921 = DIRECTION ( 'NONE',  ( 0.000000000000000000, 0.000000000000000000, -1.000000000000000000 ) ) ;
#4922 = CARTESIAN_POINT ( 'NONE',  ( -68.00000000218494733, 7.499999999999996447, 14.99999999999999645 ) ) ;
#4923 = CARTESIAN_POINT ( 'NONE',  ( 67.40000000109247935, 7.933012699999995476, 15.85617417291294196 ) ) ;
#4924 = AXIS2_PLACEMENT_3D ( 'NONE', #18831, #5660, #9169 ) ;
#4925 = CARTESIAN_POINT ( 'NONE',  ( -2.000000000000001776, 0.000000000000000000, 0.000000000000000000 ) ) ;
#4926 = CIRCLE ( 'NONE', #20591, 6.499999999999999112 ) ;
#4927 = CARTESIAN_POINT ( 'NONE',  ( -68.79999999999999716, 8.232233047033629347, 13.23223304703362402 ) ) ;
#4928 = FACE_BOUND ( 'NONE', #19113, .T. ) ;
#4929 = CARTESIAN_POINT ( 'NONE',  ( 60.00000000000000000, 13.23725887712638283, 12.63247214140022123 ) ) ;
#4930 = EDGE_CURVE ( 'NONE', #23288, #2408, #1186, .T. ) ;
#4931 = VECTOR ( 'NONE', #14871, 1000.000000000000000 ) ;
#4932 = CARTESIAN_POINT ( 'NONE',  ( 3.458734125000000770, 1.432654583217640498, 1.550000001365597013 ) ) ;
#4933 = CARTESIAN_POINT ( 'NONE',  ( 1.656854249492384135, -3.999999999999999112, 13.31250000000001243 ) ) ;
#4934 = CARTESIAN_POINT ( 'NONE',  ( 27.50000000000000000, 7.500000000000002665, -36.31025403784445160 ) ) ;
#4935 = CARTESIAN_POINT ( 'NONE',  ( -1.656854249492379250, 4.000000000000000000, 9.937500002731198379 ) ) ;
#4936 = CARTESIAN_POINT ( 'NONE',  ( 4.197393957002303999, 0.8151795401431359833, -3.503767560748935139 ) ) ;
#4937 = ORIENTED_EDGE ( 'NONE', *, *, #22701, .F. ) ;
#4938 = LINE ( 'NONE', #13946, #2073 ) ;
#4939 = VERTEX_POINT ( 'NONE', #10089 ) ;
#4940 = CARTESIAN_POINT ( 'NONE',  ( 60.24768183416157541, 7.123453452023678523, 17.78030770151605822 ) ) ;
#4941 = CARTESIAN_POINT ( 'NONE',  ( -68.50000000109247367, 10.85617417291294551, 12.93301269999999370 ) ) ;
#4942 = AXIS2_PLACEMENT_3D ( 'NONE', #14621, #206, #9339 ) ;
#4943 = AXIS2_PLACEMENT_3D ( 'NONE', #2144, #10, #16778 ) ;
#4944 = EDGE_CURVE ( 'NONE', #3850, #17912, #8522, .T. ) ;
#4945 = DIRECTION ( 'NONE',  ( 1.000000000000000000, 0.000000000000000000, 0.000000000000000000 ) ) ;
#4946 = VERTEX_POINT ( 'NONE', #17378 ) ;
#4947 = FACE_OUTER_BOUND ( 'NONE', #11013, .T. ) ;
#4948 = CIRCLE ( 'NONE', #13382, 6.500000000000000888 ) ;
#4949 = VERTEX_POINT ( 'NONE', #2860 ) ;
#4950 = DIRECTION ( 'NONE',  ( 0.000000000000000000, -1.000000000000000000, -1.040834085586083783E-14 ) ) ;
#4951 = EDGE_LOOP ( 'NONE', ( #21129, #15799, #1189, #3435 ) ) ;
#4952 = CARTESIAN_POINT ( 'NONE',  ( 51.50231816583844591, 12.78030770151603868, 12.12345345202365188 ) ) ;
#4953 = AXIS2_PLACEMENT_3D ( 'NONE', #19656, #21814, #10946 ) ;
#4954 = CARTESIAN_POINT ( 'NONE',  ( -68.40000000218495302, 12.50000000000000000, 14.99999999999999645 ) ) ;
#4955 = PRESENTATION_LAYER_ASSIGNMENT (  '', '', ( #8032 ) ) ;
#4956 = DIRECTION ( 'NONE',  ( 0.000000000000000000, 0.000000000000000000, 1.000000000000000000 ) ) ;
#4957 = DIRECTION ( 'NONE',  ( -0.000000000000000000, -1.000000000000000000, -0.000000000000000000 ) ) ;
#4958 =( BOUNDED_CURVE ( )  B_SPLINE_CURVE ( 2, ( #823, #6466, #17605, #4542, #19370, #1170, #22737, #6348, #10436 ),
 .UNSPECIFIED., .F., .F. ) 
 B_SPLINE_CURVE_WITH_KNOTS ( ( 3, 2, 2, 2, 3 ),
 ( 0.05000000000000000278, 0.06250000000000000000, 0.07499999999999999722, 0.08749999999999999445, 0.1000000000000000056 ),
 .UNSPECIFIED. ) 
 CURVE ( )  GEOMETRIC_REPRESENTATION_ITEM ( )  RATIONAL_B_SPLINE_CURVE ( ( 1.000000000000000000, 0.9238795325112867385, 1.000000000000000000, 0.9238795325112867385, 1.000000000000000000, 0.9238795325112867385, 1.000000000000000000, 0.9238795325112867385, 1.000000000000000000 ) ) 
 REPRESENTATION_ITEM ( '' )  );
#4959 = CARTESIAN_POINT ( 'NONE',  ( -1.432654583217639166, 3.458734125000000770, 14.50000000136560629 ) ) ;
#4960 = CARTESIAN_POINT ( 'NONE',  ( 4.000000000000000000, 4.898587196589412829E-16, -2.074999997268812013 ) ) ;
#4961 = VECTOR ( 'NONE', #2265, 1000.000000000000114 ) ;
#4962 = LINE ( 'NONE', #14077, #8555 ) ;
#4963 = PLANE ( 'NONE',  #3698 ) ;
#4964 = AXIS2_PLACEMENT_3D ( 'NONE', #21250, #4867, #12202 ) ;
#4965 = EDGE_CURVE ( 'NONE', #611, #13486, #948, .T. ) ;
#4966 = CARTESIAN_POINT ( 'NONE',  ( 50.75231816583844591, 7.926799079670502124, 17.16943976678978245 ) ) ;
#4967 = ADVANCED_FACE ( 'NONE', ( #6482 ), #718, .T. ) ;
#4968 = CARTESIAN_POINT ( 'NONE',  ( -2.445694354108820523, 2.445694354108820523, 0.8625000013655955700 ) ) ;
#4969 = DIRECTION ( 'NONE',  ( -1.000000000000000000, 0.000000000000000000, 0.000000000000000000 ) ) ;
#4970 = ORIENTED_EDGE ( 'NONE', *, *, #15696, .T. ) ;
#4971 = CARTESIAN_POINT ( 'NONE',  ( 20.00000000000000355, 4.500000000000003553, -2.449293598294706907E-15 ) ) ;
#4972 = DIRECTION ( 'NONE',  ( -1.000000000000000000, -0.000000000000000000, 0.000000000000000000 ) ) ;
#4973 = ORIENTED_EDGE ( 'NONE', *, *, #3043, .F. ) ;
#4974 = CARTESIAN_POINT ( 'NONE',  ( 12.68853974071656232, -8.974600000000002353, 5.000000000000079936 ) ) ;
#4975 = CIRCLE ( 'NONE', #20236, 8.749000000000002331 ) ;
#4976 = CARTESIAN_POINT ( 'NONE',  ( -4.000000000000000000, -1.656854249492383246, -1.512499997268811347 ) ) ;
#4977 = EDGE_CURVE ( 'NONE', #20778, #14063, #6239, .T. ) ;
#4978 = ORIENTED_EDGE ( 'NONE', *, *, #10808, .F. ) ;
#4979 = ADVANCED_FACE ( 'NONE', ( #15480 ), #21060, .T. ) ;
#4980 = VERTEX_POINT ( 'NONE', #19271 ) ;
#4981 = CARTESIAN_POINT ( 'NONE',  ( 1.065083781909167415, -6.890627091270381754, -0.2578475836320779924 ) ) ;
#4982 = CARTESIAN_POINT ( 'NONE',  ( 15.00195451966726523, -11.25000000000000355, 5.000000000000079936 ) ) ;
#4983 = ORIENTED_EDGE ( 'NONE', *, *, #8082, .T. ) ;
#4984 = CARTESIAN_POINT ( 'NONE',  ( 4.235886605889389145, 2.417314728048528760, -3.751161874094018245 ) ) ;
#4985 = AXIS2_PLACEMENT_3D ( 'NONE', #6617, #15390, #13471 ) ;
#4986 = UNCERTAINTY_MEASURE_WITH_UNIT (LENGTH_MEASURE( 1.000000000000000082E-05 ), #15162, 'distance_accuracy_value', 'NONE');
#4987 = CYLINDRICAL_SURFACE ( 'NONE', #14059, 2.500000000000002220 ) ;
#4988 = ORIENTED_EDGE ( 'NONE', *, *, #19938, .F. ) ;
#4989 = CARTESIAN_POINT ( 'NONE',  ( 65.65000000109247935, 9.999999999999998224, 17.06698730000000097 ) ) ;
#4990 = VECTOR ( 'NONE', #22447, 1000.000000000000000 ) ;
#4991 = CIRCLE ( 'NONE', #1143, 2.499999999999998668 ) ;
#4992 = CARTESIAN_POINT ( 'NONE',  ( 66.50000000109245946, 12.06698730000000275, 15.85617417291294196 ) ) ;
#4993 = DIRECTION ( 'NONE',  ( -1.000000000000000000, 0.000000000000000000, 0.000000000000000000 ) ) ;
#4994 = PLANE ( 'NONE',  #10743 ) ;
#4995 = CARTESIAN_POINT ( 'NONE',  ( 58.72106816583844591, 14.02818770551465377, 16.58880310854672757 ) ) ;
#4996 = EDGE_CURVE ( 'NONE', #16693, #8676, #18626, .T. ) ;
#4997 = CARTESIAN_POINT ( 'NONE',  ( 2.445694354108820523, -2.445694354108820079, 5.112500001365595459 ) ) ;
#4998 = CARTESIAN_POINT ( 'NONE',  ( -3.458734124999998105, 1.432654583217640276, 15.37500000136560807 ) ) ;
#4999 = CARTESIAN_POINT ( 'NONE',  ( 30.70991776966726405, -11.25000000000000355, 5.000000000000079936 ) ) ;
#5000 = CARTESIAN_POINT ( 'NONE',  ( 17.25467643033275067, -11.25000000000000355, 5.000000000000079936 ) ) ;
#5001 = ORIENTED_EDGE ( 'NONE', *, *, #14664, .F. ) ;
#5002 = CARTESIAN_POINT ( 'NONE',  ( 4.999999999999999112, -10.82112760146734765, -1.975651141462353211 ) ) ;
#5003 = DIRECTION ( 'NONE',  ( -0.000000000000000000, 0.000000000000000000, 1.000000000000000000 ) ) ;
#5004 = DIRECTION ( 'NONE',  ( 0.000000000000000000, 0.000000000000000000, 1.000000000000000000 ) ) ;
#5005 = VECTOR ( 'NONE', #19399, 1000.000000000000114 ) ;
#5006 = ADVANCED_FACE ( 'NONE', ( #15212 ), #23528, .F. ) ;
#5007 = ORIENTED_EDGE ( 'NONE', *, *, #23465, .F. ) ;
#5008 = DIRECTION ( 'NONE',  ( 0.000000000000000000, 0.000000000000000000, 1.000000000000000000 ) ) ;
#5009 = CARTESIAN_POINT ( 'NONE',  ( 71.75000000109248788, 11.46158073645647235, 13.53841926354352232 ) ) ;
#5010 = CARTESIAN_POINT ( 'NONE',  ( 59.62500000000000711, 12.82842712474620228, 17.82842712474617386 ) ) ;
#5011 = ORIENTED_EDGE ( 'NONE', *, *, #14342, .F. ) ;
#5012 = CARTESIAN_POINT ( 'NONE',  ( 66.10000000218495586, 11.76776695296636888, 16.76776695296636532 ) ) ;
#5013 = ORIENTED_EDGE ( 'NONE', *, *, #21248, .F. ) ;
#5014 = CARTESIAN_POINT ( 'NONE',  ( 57.97106816583845301, 5.971812294485345340, 13.41119689145326710 ) ) ;
#5015 = CARTESIAN_POINT ( 'NONE',  ( 67.40000000218495302, 9.999999999999998224, 12.49999999999999289 ) ) ;
#5016 = LINE ( 'NONE', #22852, #14549 ) ;
#5017 = DIRECTION ( 'NONE',  ( 0.000000000000000000, 0.000000000000000000, -1.000000000000000000 ) ) ;
#5018 = CARTESIAN_POINT ( 'NONE',  ( 67.10000000109246798, 10.85617417291294551, 12.93301269999999192 ) ) ;
#5019 = EDGE_LOOP ( 'NONE', ( #10948, #2490, #2747, #14151 ) ) ;
#5020 = AXIS2_PLACEMENT_3D ( 'NONE', #15365, #4434, #6236 ) ;
#5021 = LINE ( 'NONE', #12350, #5319 ) ;
#5022 = CYLINDRICAL_SURFACE ( 'NONE', #7250, 4.000000000000001776 ) ;
#5023 = CARTESIAN_POINT ( 'NONE',  ( 67.80000000109247082, 9.143825827087050939, 12.93301269999999370 ) ) ;
#5024 = CARTESIAN_POINT ( 'NONE',  ( -3.458734124999999437, 0.000000000000000000, 18.68750000136560629 ) ) ;
#5025 = CARTESIAN_POINT ( 'NONE',  ( 49.55947366966726264, -11.25000000000000355, 10.00000000000008882 ) ) ;
#5026 = CARTESIAN_POINT ( 'NONE',  ( 14.99999999999995914, -15.00000000000000000, -20.00000000000000355 ) ) ;
#5027 = ORIENTED_EDGE ( 'NONE', *, *, #23127, .F. ) ;
#5028 = CARTESIAN_POINT ( 'NONE',  ( -2.828427124746190291, 2.828427124746190291, -1.824999999999998401 ) ) ;
#5029 = CARTESIAN_POINT ( 'NONE',  ( 56.81250000000000000, 13.00000000000000000, 14.99999999999998757 ) ) ;
#5030 = CARTESIAN_POINT ( 'NONE',  ( -1.800000000000000711, 0.000000000000000000, 0.000000000000000000 ) ) ;
#5031 = EDGE_CURVE ( 'NONE', #1981, #22779, #22116, .T. ) ;
#5032 = ORIENTED_EDGE ( 'NONE', *, *, #15085, .F. ) ;
#5033 = CARTESIAN_POINT ( 'NONE',  ( 0.000000000000000000, -4.762163868918344534, 9.915734732513202587 ) ) ;
#5034 = CARTESIAN_POINT ( 'NONE',  ( 1.432654583217639832, 3.458734125000000326, -0.5749999986344046521 ) ) ;
#5035 = DIRECTION ( 'NONE',  ( 0.000000000000000000, 0.000000000000000000, 1.000000000000000000 ) ) ;
#5036 = ORIENTED_EDGE ( 'NONE', *, *, #18988, .F. ) ;
#5037 = DIRECTION ( 'NONE',  ( 0.000000000000000000, 0.000000000000000000, 1.000000000000000000 ) ) ;
#5038 = ORIENTED_EDGE ( 'NONE', *, *, #5686, .F. ) ;
#5039 = PLANE ( 'NONE',  #9894 ) ;
#5040 = ORIENTED_EDGE ( 'NONE', *, *, #6266, .F. ) ;
#5041 = CARTESIAN_POINT ( 'NONE',  ( -3.458734124999998993, -1.432654583217642497, 14.75000000136560452 ) ) ;
#5042 = CARTESIAN_POINT ( 'NONE',  ( -4.000000000000000000, 0.1981133338132459731, 2.096406544454392723E-17 ) ) ;
#5043 = DIRECTION ( 'NONE',  ( -1.000000000000000000, 0.000000000000000000, 0.000000000000000000 ) ) ;
#5044 = CARTESIAN_POINT ( 'NONE',  ( 2.000000000000001776, 0.000000000000000000, 0.000000000000000000 ) ) ;
#5045 = CARTESIAN_POINT ( 'NONE',  ( -69.99999999999998579, 11.76776695296636888, 16.76776695296636532 ) ) ;
#5046 = DIRECTION ( 'NONE',  ( 0.000000000000000000, 0.000000000000000000, 1.000000000000000000 ) ) ;
#5047 = CARTESIAN_POINT ( 'NONE',  ( 60.00000000000002132, 13.01044786497014805, 14.65336842865874267 ) ) ;
#5048 = CARTESIAN_POINT ( 'NONE',  ( 1.432654583217640276, 3.458734125000000770, 0.6750000013655963471 ) ) ;
#5049 = CARTESIAN_POINT ( 'NONE',  ( 19.99999999999999645, 1.500000000000003109, -50.00000000000000000 ) ) ;
#5050 = CARTESIAN_POINT ( 'NONE',  ( -3.251184232703611343, 2.330193357860981251, -3.674599999999999866 ) ) ;
#5051 = CARTESIAN_POINT ( 'NONE',  ( -2.445694354108818303, -2.445694354108820523, 18.56250000136560629 ) ) ;
#5052 = PLANE ( 'NONE',  #14575 ) ;
#5053 = EDGE_LOOP ( 'NONE', ( #6751, #5225, #346, #14833 ) ) ;
#5054 = CARTESIAN_POINT ( 'NONE',  ( -71.40000000109249356, 7.933012699999995476, 15.85617417291294196 ) ) ;
#5055 = ORIENTED_EDGE ( 'NONE', *, *, #20495, .T. ) ;
#5056 = CARTESIAN_POINT ( 'NONE',  ( 53.49768183416157541, 12.16943976678977535, 12.92679907967048614 ) ) ;
#5057 = CARTESIAN_POINT ( 'NONE',  ( -67.55000000109247082, 8.538419263543524096, 13.53841926354352054 ) ) ;
#5058 = DIRECTION ( 'NONE',  ( 0.000000000000000000, 0.000000000000000000, -1.000000000000000000 ) ) ;
#5059 = CARTESIAN_POINT ( 'NONE',  ( -3.458734125000000326, 0.000000000000000000, -3.262499998634404541 ) ) ;
#5060 = ORIENTED_EDGE ( 'NONE', *, *, #4249, .T. ) ;
#5061 = CARTESIAN_POINT ( 'NONE',  ( 1.236993788156008760E-15, 0.000000000000000000, 21.31370849898476649 ) ) ;
#5062 = ORIENTED_EDGE ( 'NONE', *, *, #9563, .F. ) ;
#5063 = VECTOR ( 'NONE', #22963, 999.9999999999997726 ) ;
#5064 = DIRECTION ( 'NONE',  ( 0.000000000000000000, -0.4999999999999993339, 0.8660254037844390407 ) ) ;
#5065 = VERTEX_POINT ( 'NONE', #20322 ) ;
#5066 = CARTESIAN_POINT ( 'NONE',  ( 57.50231816583843170, 12.07320092032949610, 12.83056023321021044 ) ) ;
#5067 = EDGE_CURVE ( 'NONE', #3140, #18283, #2259, .T. ) ;
#5068 = CARTESIAN_POINT ( 'NONE',  ( -67.55000000218494449, 12.50000000000000000, 13.96446609406725869 ) ) ;
#5069 = LINE ( 'NONE', #12402, #18256 ) ;
#5070 = CARTESIAN_POINT ( 'NONE',  ( 4.999999999999997335, 3.872983346207417021, -1.000000000000000000 ) ) ;
#5071 = CARTESIAN_POINT ( 'NONE',  ( 2.445694354108822299, -2.445694354108820079, 16.06250000136560629 ) ) ;
#5072 = CARTESIAN_POINT ( 'NONE',  ( -1.656854249492379250, 4.000000000000000000, 10.93750000273119483 ) ) ;
#5073 = EDGE_CURVE ( 'NONE', #22188, #16559, #22608, .T. ) ;
#5074 = CARTESIAN_POINT ( 'NONE',  ( 56.25000000000000711, 7.878679656440361612, 17.12132034355964549 ) ) ;
#5075 = CARTESIAN_POINT ( 'NONE',  ( 2.500000000000000000, 2.357898499370431722, -2.818925648462311528E-15 ) ) ;
#5076 = CARTESIAN_POINT ( 'NONE',  ( 51.59606816583843170, 11.17458954617364242, 11.97181229448534800 ) ) ;
#5077 = CARTESIAN_POINT ( 'NONE',  ( 3.458734125000000770, 4.235727675282972223E-16, 1.487500001365596125 ) ) ;
#5078 = CARTESIAN_POINT ( 'NONE',  ( 30.70991776966726405, -11.25000000000000355, 10.00000000000008882 ) ) ;
#5079 = EDGE_LOOP ( 'NONE', ( #8233, #613, #14087, #10915, #5013, #4139, #13147, #21089, #12455, #13370, #19073, #20361, #15781, #17713, #21440, #9630 ) ) ;
#5080 = DIRECTION ( 'NONE',  ( 0.000000000000000000, 0.000000000000000000, 1.000000000000000000 ) ) ;
#5081 = CARTESIAN_POINT ( 'NONE',  ( -27.50000000000000711, 4.500000000000003553, -33.66025403784446723 ) ) ;
#5082 = ORIENTED_EDGE ( 'NONE', *, *, #15357, .F. ) ;
#5083 = CARTESIAN_POINT ( 'NONE',  ( 58.59375000000000711, 11.24264068711927322, 11.99999999999998934 ) ) ;
#5084 = CARTESIAN_POINT ( 'NONE',  ( 1.656854249492380360, 4.000000000000000000, 2.112500002731187987 ) ) ;
#5085 = CARTESIAN_POINT ( 'NONE',  ( -5.555405146766188906, -9.000000000000003553, 5.000000000000079936 ) ) ;
#5086 = ORIENTED_EDGE ( 'NONE', *, *, #12623, .T. ) ;
#5087 = ORIENTED_EDGE ( 'NONE', *, *, #3832, .T. ) ;
#5088 = DIRECTION ( 'NONE',  ( -1.000000000000000000, -0.000000000000000000, -0.000000000000000000 ) ) ;
#5089 = DIRECTION ( 'NONE',  ( 0.000000000000000000, 0.000000000000000000, 1.000000000000000000 ) ) ;
#5090 = ORIENTED_EDGE ( 'NONE', *, *, #6410, .F. ) ;
#5091 = DIRECTION ( 'NONE',  ( 0.3420201433256622181, 0.9396926207859107594, -6.162975822039141593E-32 ) ) ;
#5092 = EDGE_CURVE ( 'NONE', #19833, #4626, #14138, .T. ) ;
#5093 = FACE_OUTER_BOUND ( 'NONE', #18401, .T. ) ;
#5094 =( BOUNDED_CURVE ( )  B_SPLINE_CURVE ( 2, ( #10139, #21105, #13496, #11819, #12053, #19093, #13727, #20989, #11587, #20756, #15648, #6647, #4720, #6409, #15416, #644, #4608, #19209, #19319, #17431, #9901, #18970, #8328, #2908, #10255, #17548, #772, #4363, #11700, #2686, #10027, #1112, #8458, #15765, #13960, #17889, #19791, #21458, #10494, #18013, #7120, #21699, #12165, #19555, #14316, #16219, #8926, #12292, #23631, #3513, #4834, #19669, #10736, #14433, #16108, #1588, #19436, #21575, #5071, #3274, #23506, #23147, #1346, #10381, #8682, #23392, #3391, #15873, #21219, #1466, #15983, #6759, #21339, #23271, #3033, #17666, #17775, #5310, #12650, #10617, #12404, #7244, #14075, #4959, #3150, #18122, #1701, #1227, #8810, #14199, #6996, #6878, #8565, #5188, #12529, #19910, #10846, #9045, #16335, #7364, #5427, #20258, #16809, #257, #16565, #18360, #22041, #9168, #2174, #34, #7477, #3979, #12764, #11316, #1941, #20128, #3863, #3734, #20016, #9280, #18472, #18591, #389, #7720, #12873, #9511, #5659, #7591, #12994, #15033, #16455, #14913, #22290, #22171, #14672, #14560, #21933, #5541, #5785, #21824, #1818, #3618, #11198, #2050, #11074, #9392, #16686, #13114, #10958 ),
 .UNSPECIFIED., .F., .F. ) 
 B_SPLINE_CURVE_WITH_KNOTS ( ( 3, 2, 2, 2, 2, 2, 2, 2, 2, 2, 2, 2, 2, 2, 2, 2, 2, 2, 2, 2, 2, 2, 2, 2, 2, 2, 2, 2, 2, 2, 2, 2, 2, 2, 2, 2, 2, 2, 2, 2, 2, 2, 2, 2, 2, 2, 2, 2, 2, 2, 2, 2, 2, 2, 2, 2, 2, 2, 2, 2, 2, 2, 2, 2, 2, 2, 2, 2, 2, 2, 2, 2, 2, 2, 3 ),
 ( 0.000000000000000000, 0.01250000000000000069, 0.02500000000000000139, 0.03749999999999999861, 0.05000000000000000278, 0.06250000000000000000, 0.07499999999999999722, 0.08749999999999999445, 0.1000000000000000056, 0.1125000000000000028, 0.1250000000000000000, 0.1375000000000000111, 0.1499999999999999944, 0.1625000000000000056, 0.1749999999999999889, 0.1875000000000000278, 0.2000000000000000111, 0.2124999999999999944, 0.2250000000000000056, 0.2374999999999999889, 0.2500000000000000000, 0.2625000000000000111, 0.2750000000000000222, 0.2874999999999999778, 0.2999999999999999889, 0.3125000000000000000, 0.3250000000000000111, 0.3375000000000000777, 0.3499999999999999778, 0.3624999999999999889, 0.3750000000000000555, 0.3875000000000000111, 0.4000000000000000222, 0.4124999999999999223, 0.4249999999999999889, 0.4375000000000000000, 0.4500000000000000111, 0.4625000000000000222, 0.4749999999999999778, 0.4874999999999999889, 0.5000000000000000000, 0.5124999999999999556, 0.5250000000000000222, 0.5374999999999999778, 0.5500000000000000444, 0.5625000000000000000, 0.5749999999999999556, 0.5875000000000000222, 0.5999999999999999778, 0.6125000000000000444, 0.6250000000000000000, 0.6374999999999999556, 0.6500000000000000222, 0.6624999999999999778, 0.6750000000000001554, 0.6875000000000000000, 0.6999999999999999556, 0.7125000000000001332, 0.7249999999999999778, 0.7375000000000000444, 0.7500000000000001110, 0.7624999999999999556, 0.7750000000000000222, 0.7874999999999998668, 0.8000000000000000444, 0.8125000000000000000, 0.8249999999999998446, 0.8375000000000000222, 0.8499999999999999778, 0.8625000000000000444, 0.8750000000000000000, 0.8874999999999999556, 0.9000000000000000222, 0.9124999999999999778, 0.9250000000000000444 ),
 .UNSPECIFIED. ) 
 CURVE ( )  GEOMETRIC_REPRESENTATION_ITEM ( )  RATIONAL_B_SPLINE_CURVE ( ( 1.000000000000000000, 0.9238795325112867385, 1.000000000000000000, 0.9238795325112867385, 1.000000000000000000, 0.9238795325112867385, 1.000000000000000000, 0.9238795325112867385, 1.000000000000000000, 0.9238795325112867385, 1.000000000000000000, 0.9238795325112867385, 1.000000000000000000, 0.9238795325112867385, 1.000000000000000000, 0.9238795325112867385, 1.000000000000000000, 0.9238795325112867385, 1.000000000000000000, 0.9238795325112867385, 1.000000000000000000, 0.9238795325112867385, 1.000000000000000000, 0.9238795325112867385, 1.000000000000000000, 0.9238795325112867385, 1.000000000000000000, 0.9238795325112867385, 1.000000000000000000, 0.9238795325112867385, 1.000000000000000000, 0.9238795325112867385, 1.000000000000000000, 0.9238795325112867385, 1.000000000000000000, 0.9238795325112867385, 1.000000000000000000, 0.9238795325112867385, 1.000000000000000000, 0.9238795325112867385, 1.000000000000000000, 0.9238795325112867385, 1.000000000000000000, 0.9238795325112867385, 1.000000000000000000, 0.9238795325112867385, 1.000000000000000000, 0.9238795325112867385, 1.000000000000000000, 0.9238795325112867385, 1.000000000000000000, 0.9238795325112867385, 1.000000000000000000, 0.9238795325112867385, 1.000000000000000000, 0.9238795325112867385, 1.000000000000000000, 0.9238795325112867385, 1.000000000000000000, 0.9238795325112867385, 1.000000000000000000, 0.9238795325112867385, 1.000000000000000000, 0.9238795325112867385, 1.000000000000000000, 0.9238795325112867385, 1.000000000000000000, 0.9238795325112867385, 1.000000000000000000, 0.9238795325112867385, 1.000000000000000000, 0.9238795325112867385, 1.000000000000000000, 0.9238795325112867385, 1.000000000000000000, 0.9238795325112867385, 1.000000000000000000, 0.9238795325112867385, 1.000000000000000000, 0.9238795325112867385, 1.000000000000000000, 0.9238795325112867385, 1.000000000000000000, 0.9238795325112867385, 1.000000000000000000, 0.9238795325112867385, 1.000000000000000000, 0.9238795325112867385, 1.000000000000000000, 0.9238795325112867385, 1.000000000000000000, 0.9238795325112867385, 1.000000000000000000, 0.9238795325112867385, 1.000000000000000000, 0.9238795325112867385, 1.000000000000000000, 0.9238795325112867385, 1.000000000000000000, 0.9238795325112867385, 1.000000000000000000, 0.9238795325112867385, 1.000000000000000000, 0.9238795325112867385, 1.000000000000000000, 0.9238795325112867385, 1.000000000000000000, 0.9238795325112867385, 1.000000000000000000, 0.9238795325112867385, 1.000000000000000000, 0.9238795325112867385, 1.000000000000000000, 0.9238795325112867385, 1.000000000000000000, 0.9238795325112867385, 1.000000000000000000, 0.9238795325112867385, 1.000000000000000000, 0.9238795325112867385, 1.000000000000000000, 0.9238795325112867385, 1.000000000000000000, 0.9238795325112867385, 1.000000000000000000, 0.9238795325112867385, 1.000000000000000000, 0.9238795325112867385, 1.000000000000000000, 0.9238795325112867385, 1.000000000000000000, 0.9238795325112867385, 1.000000000000000000, 0.9238795325112867385, 1.000000000000000000, 0.9238795325112867385, 1.000000000000000000, 0.9238795325112867385, 1.000000000000000000, 0.9238795325112867385, 1.000000000000000000, 0.9238795325112867385, 1.000000000000000000, 0.9238795325112867385, 1.000000000000000000, 0.9238795325112867385, 1.000000000000000000, 0.9238795325112867385, 1.000000000000000000 ) ) 
 REPRESENTATION_ITEM ( '' )  );
#5095 = ADVANCED_FACE ( 'NONE', ( #2598 ), #22478, .F. ) ;
#5096 = ORIENTED_EDGE ( 'NONE', *, *, #21430, .F. ) ;
#5097 = FACE_OUTER_BOUND ( 'NONE', #163, .T. ) ;
#5098 = VECTOR ( 'NONE', #5848, 1000.000000000000000 ) ;
#5099 = CARTESIAN_POINT ( 'NONE',  ( 71.50000000000000000, 12.50000000000000000, 14.99999999999999645 ) ) ;
#5100 = CIRCLE ( 'NONE', #14689, 6.543750000000017053 ) ;
#5101 = EDGE_CURVE ( 'NONE', #22551, #19381, #20478, .T. ) ;
#5102 = DIRECTION ( 'NONE',  ( 0.000000000000000000, -1.000000000000000000, -0.000000000000000000 ) ) ;
#5103 = CARTESIAN_POINT ( 'NONE',  ( 19.99999999999998934, 9.999999999999966249, -50.00000000000000000 ) ) ;
#5104 = CARTESIAN_POINT ( 'NONE',  ( 51.56250000000000711, 5.999999999999996447, 15.00000000000001599 ) ) ;
#5105 = CARTESIAN_POINT ( 'NONE',  ( 1.432654583217642275, -3.458734124999999437, 2.050000001365597679 ) ) ;
#5106 = DIRECTION ( 'NONE',  ( 0.000000000000000000, 0.000000000000000000, 1.000000000000000000 ) ) ;
#5107 = CARTESIAN_POINT ( 'NONE',  ( 2.445694354108821855, -2.445694354108820079, 16.81250000136560629 ) ) ;
#5108 = CARTESIAN_POINT ( 'NONE',  ( 40.13469571966727045, -11.25000000000000355, 5.000000000000079936 ) ) ;
#5109 = CARTESIAN_POINT ( 'NONE',  ( -70.60000000218494165, 9.999999999999998224, 12.49999999999999289 ) ) ;
#5110 = ORIENTED_EDGE ( 'NONE', *, *, #14868, .F. ) ;
#5111 = CARTESIAN_POINT ( 'NONE',  ( -3.270501301980698550, -1.125461230421587633, 2.040000000000001812 ) ) ;
#5112 = CARTESIAN_POINT ( 'NONE',  ( 0.000000000000000000, -1.975651141462315463, 10.82112760146735475 ) ) ;
#5113 = CARTESIAN_POINT ( 'NONE',  ( -2.828427124746189403, -2.828427124746190735, -1.574999999999998179 ) ) ;
#5114 = EDGE_LOOP ( 'NONE', ( #16377, #16012, #14760, #10578 ) ) ;
#5115 = DIRECTION ( 'NONE',  ( 0.000000000000000000, 0.000000000000000000, 1.000000000000000000 ) ) ;
#5116 = CARTESIAN_POINT ( 'NONE',  ( 71.45000000109247651, 7.933012699999995476, 14.99999999999999645 ) ) ;
#5117 = ADVANCED_FACE ( 'NONE', ( #4291 ), #19133, .F. ) ;
#5118 = CARTESIAN_POINT ( 'NONE',  ( 50.00000000000000000, 15.00000000000004263, 34.11836509645781490 ) ) ;
#5119 = ORIENTED_EDGE ( 'NONE', *, *, #10428, .T. ) ;
#5120 = CARTESIAN_POINT ( 'NONE',  ( 4.000000000000000000, 0.000000000000000000, -3.699999999999998401 ) ) ;
#5121 = VERTEX_POINT ( 'NONE', #10061 ) ;
#5122 = CARTESIAN_POINT ( 'NONE',  ( 51.18750000000000711, 9.999999999999978684, 10.99999999999999645 ) ) ;
#5123 = EDGE_CURVE ( 'NONE', #9522, #7689, #959, .T. ) ;
#5124 = CARTESIAN_POINT ( 'NONE',  ( 68.00000000218494733, 7.499999999999996447, 14.99999999999999645 ) ) ;
#5125 = FACE_OUTER_BOUND ( 'NONE', #16038, .T. ) ;
#5126 = LINE ( 'NONE', #23449, #3732 ) ;
#5127 = EDGE_CURVE ( 'NONE', #23404, #17175, #13529, .T. ) ;
#5128 = VERTEX_POINT ( 'NONE', #2948 ) ;
#5129 = ADVANCED_FACE ( 'NONE', ( #8018 ), #21030, .F. ) ;
#5130 = DIRECTION ( 'NONE',  ( -1.000000000000000000, 0.000000000000000000, 0.000000000000000000 ) ) ;
#5131 = CARTESIAN_POINT ( 'NONE',  ( 52.56018183416157541, 7.000000000000000000, 14.93194885905437097 ) ) ;
#5132 = CYLINDRICAL_SURFACE ( 'NONE', #22529, 8.749000000000002331 ) ;
#5133 = CIRCLE ( 'NONE', #17393, 11.00000000000000000 ) ;
#5134 = CARTESIAN_POINT ( 'NONE',  ( 65.90000000109246514, 9.143825827087049163, 17.06698729999999742 ) ) ;
#5135 = CARTESIAN_POINT ( 'NONE',  ( 1.872352939448454495E-15, -3.458734125000000770, 17.93750000136560274 ) ) ;
#5136 = CARTESIAN_POINT ( 'NONE',  ( 19.99999999999999645, 4.500000000000003553, -50.00000000000000000 ) ) ;
#5137 = CARTESIAN_POINT ( 'NONE',  ( 68.89999999999999147, 9.999999999999998224, 12.49999999999999289 ) ) ;
#5138 = ORIENTED_EDGE ( 'NONE', *, *, #27, .T. ) ;
#5139 = CARTESIAN_POINT ( 'NONE',  ( 2.828427124746189847, 2.828427124746190291, -2.074999999999998845 ) ) ;
#5140 = CARTESIAN_POINT ( 'NONE',  ( 57.46875000000000711, 6.999999999999992006, 13.75735931288071967 ) ) ;
#5141 = FACE_OUTER_BOUND ( 'NONE', #861, .T. ) ;
#5142 = VERTEX_POINT ( 'NONE', #22719 ) ;
#5143 = CARTESIAN_POINT ( 'NONE',  ( 2.500000000000000000, 0.000000000000000000, 0.000000000000000000 ) ) ;
#5144 = CARTESIAN_POINT ( 'NONE',  ( 1.432654583217639832, 3.458734125000000326, -2.574999998634404541 ) ) ;
#5145 = CARTESIAN_POINT ( 'NONE',  ( -65.85000000109246798, 9.999999999999998224, 17.06698730000000097 ) ) ;
#5146 = AXIS2_PLACEMENT_3D ( 'NONE', #5081, #8694, #9054 ) ;
#5147 = VERTEX_POINT ( 'NONE', #918 ) ;
#5148 = DIRECTION ( 'NONE',  ( 0.000000000000000000, 0.000000000000000000, 1.000000000000000000 ) ) ;
#5149 = VERTEX_POINT ( 'NONE', #6332 ) ;
#5150 = LINE ( 'NONE', #8890, #7206 ) ;
#5151 = ORIENTED_EDGE ( 'NONE', *, *, #7527, .T. ) ;
#5152 = CARTESIAN_POINT ( 'NONE',  ( 9.920644283265380691E-16, 4.000000000000000000, 19.75000000000001066 ) ) ;
#5153 = DIRECTION ( 'NONE',  ( 0.000000000000000000, -0.000000000000000000, 1.000000000000000000 ) ) ;
#5154 = CARTESIAN_POINT ( 'NONE',  ( 5.000000000000000000, 0.000000000000000000, 0.000000000000000000 ) ) ;
#5155 = ADVANCED_FACE ( 'NONE', ( #1038 ), #9805, .T. ) ;
#5156 = CARTESIAN_POINT ( 'NONE',  ( 12.00000000000000000, 0.000000000000000000, -4.000000000000001776 ) ) ;
#5157 = VECTOR ( 'NONE', #19980, 1000.000000000000000 ) ;
#5158 = EDGE_CURVE ( 'NONE', #22418, #17065, #5186, .T. ) ;
#5159 = AXIS2_PLACEMENT_3D ( 'NONE', #1777, #5262, #11031 ) ;
#5160 = CARTESIAN_POINT ( 'NONE',  ( -70.74999999999998579, 12.50000000000000000, 16.03553390593273420 ) ) ;
#5161 = AXIS2_PLACEMENT_3D ( 'NONE', #15717, #8627, #6950 ) ;
#5162 = DIRECTION ( 'NONE',  ( -0.000000000000000000, -0.000000000000000000, 1.000000000000000000 ) ) ;
#5163 = PLANE ( 'NONE',  #20370 ) ;
#5164 = CARTESIAN_POINT ( 'NONE',  ( -2.117863837641485618E-16, 3.458734125000000770, -0.2624999986344037084 ) ) ;
#5165 = CARTESIAN_POINT ( 'NONE',  ( 67.20000000218495018, 7.499999999999996447, 14.99999999999999645 ) ) ;
#5166 = CARTESIAN_POINT ( 'NONE',  ( -1.027321559264960715, 3.880635692936085679, 9.999401128100736003 ) ) ;
#5167 = CARTESIAN_POINT ( 'NONE',  ( 2.445694354108821411, 2.445694354108820523, 17.06250000136560629 ) ) ;
#5168 = CARTESIAN_POINT ( 'NONE',  ( -19.99999999999999645, -9.000000000000003553, 5.000000000000079936 ) ) ;
#5169 =( REPRESENTATION_RELATIONSHIP ('NONE','NONE', #8403, #10226 ) REPRESENTATION_RELATIONSHIP_WITH_TRANSFORMATION ( #2986 )SHAPE_REPRESENTATION_RELATIONSHIP( ) );
#5170 = VERTEX_POINT ( 'NONE', #15574 ) ;
#5171 = CARTESIAN_POINT ( 'NONE',  ( -3.999999999999999112, 0.000000000000000000, 14.12500000273119660 ) ) ;
#5172 = ORIENTED_EDGE ( 'NONE', *, *, #11592, .F. ) ;
#5173 = CARTESIAN_POINT ( 'NONE',  ( 55.56018183416157541, 5.999999999999996447, 14.93194885905437808 ) ) ;
#5174 = CARTESIAN_POINT ( 'NONE',  ( -67.50000000109247367, 7.933012699999995476, 14.14382582708705094 ) ) ;
#5175 = DIRECTION ( 'NONE',  ( 0.000000000000000000, 0.000000000000000000, 1.000000000000000000 ) ) ;
#5176 = ORIENTED_EDGE ( 'NONE', *, *, #16388, .F. ) ;
#5177 = CARTESIAN_POINT ( 'NONE',  ( 6.405354440716562792, -8.974600000000002353, 5.000000000000079936 ) ) ;
#5178 = AXIS2_PLACEMENT_3D ( 'NONE', #17907, #7135, #1484 ) ;
#5179 = ORIENTED_EDGE ( 'NONE', *, *, #18587, .F. ) ;
#5180 = DIRECTION ( 'NONE',  ( -0.5000000000000013323, 0.000000000000000000, -0.8660254037844380415 ) ) ;
#5181 = ORIENTED_EDGE ( 'NONE', *, *, #6695, .T. ) ;
#5182 = CARTESIAN_POINT ( 'NONE',  ( 50.37731816583844591, 7.830560233210212218, 12.92679907967049679 ) ) ;
#5183 = CARTESIAN_POINT ( 'NONE',  ( -68.50000000218494733, 11.76776695296636888, 16.76776695296636532 ) ) ;
#5184 = DIRECTION ( 'NONE',  ( -7.087422195345011518E-32, -1.000000000000000000, -0.000000000000000000 ) ) ;
#5185 = CIRCLE ( 'NONE', #18570, 4.000000000000001776 ) ;
#5186 = CIRCLE ( 'NONE', #8270, 2.041999999999999815 ) ;
#5187 = FACE_OUTER_BOUND ( 'NONE', #13595, .T. ) ;
#5188 = CARTESIAN_POINT ( 'NONE',  ( -1.432654583217639832, -3.458734125000000326, 13.87500000136560452 ) ) ;
#5189 = CARTESIAN_POINT ( 'NONE',  ( 4.999999999999999112, 4.762163868918412923, -9.915734732513167060 ) ) ;
#5190 = CARTESIAN_POINT ( 'NONE',  ( 57.09375000000000711, 11.24264068711927322, 11.99999999999998934 ) ) ;
#5191 = DIRECTION ( 'NONE',  ( -1.000000000000000000, -0.000000000000000000, 0.000000000000000000 ) ) ;
#5192 = CARTESIAN_POINT ( 'NONE',  ( 56.34375000000000711, 8.757359312880723223, 18.00000000000000355 ) ) ;
#5193 = VECTOR ( 'NONE', #10534, 1000.000000000000000 ) ;
#5194 = CARTESIAN_POINT ( 'NONE',  ( 6.353591512924457348E-16, -3.458734125000000770, -0.7624999986344024316 ) ) ;
#5195 = CARTESIAN_POINT ( 'NONE',  ( 4.000000000000001776, -1.656854249492379694, 18.56250000273119838 ) ) ;
#5196 = CARTESIAN_POINT ( 'NONE',  ( -20.00000000000001066, 1.500000000000003109, -50.00000000000000000 ) ) ;
#5197 = ADVANCED_FACE ( 'NONE', ( #13886 ), #20687, .T. ) ;
#5198 = VERTEX_POINT ( 'NONE', #6087 ) ;
#5199 = DIRECTION ( 'NONE',  ( 0.8191520442889902442, 1.003171929053522651E-16, -0.5735764363510482688 ) ) ;
#5200 = CARTESIAN_POINT ( 'NONE',  ( -1.390230914382372118, -4.043987460488664532, -3.502507215260523665 ) ) ;
#5201 = ORIENTED_EDGE ( 'NONE', *, *, #23501, .T. ) ;
#5202 = CARTESIAN_POINT ( 'NONE',  ( 57.37500000000000000, 7.878679656440349177, 12.87867965644035984 ) ) ;
#5203 = APPLICATION_PROTOCOL_DEFINITION ( 'draft international standard', 'automotive_design', 1998, #1801 ) ;
#5204 = CARTESIAN_POINT ( 'NONE',  ( -4.000000000000000000, 0.000000000000000000, 1.425000002731187765 ) ) ;
#5205 = PLANE ( 'NONE',  #6318 ) ;
#5206 = ORIENTED_EDGE ( 'NONE', *, *, #1894, .F. ) ;
#5207 = CARTESIAN_POINT ( 'NONE',  ( 1.971781867644420635E-15, -4.000000000000000000, 15.25000000000001066 ) ) ;
#5208 = ORIENTED_EDGE ( 'NONE', *, *, #6571, .F. ) ;
#5209 = CARTESIAN_POINT ( 'NONE',  ( 2.149058192116893196, -6.264794173742287420, -0.06682554136338376971 ) ) ;
#5210 = LINE ( 'NONE', #15892, #14098 ) ;
#5211 = ORIENTED_EDGE ( 'NONE', *, *, #13057, .F. ) ;
#5212 = FACE_OUTER_BOUND ( 'NONE', #10692, .T. ) ;
#5213 = CARTESIAN_POINT ( 'NONE',  ( -3.999999999999999112, 0.000000000000000000, 12.00000000000001066 ) ) ;
#5214 = CARTESIAN_POINT ( 'NONE',  ( 4.000000000000000888, 1.563622288139206118, -0.2253451193528334950 ) ) ;
#5215 = CARTESIAN_POINT ( 'NONE',  ( 70.70000000000000284, 12.50000000000000000, 14.99999999999999645 ) ) ;
#5216 = CARTESIAN_POINT ( 'NONE',  ( -19.55556463033274284, -11.25000000000000355, 5.000000000000079936 ) ) ;
#5217 = CARTESIAN_POINT ( 'NONE',  ( 0.000000000000000000, 0.000000000000000000, -4.694516984716113228 ) ) ;
#5218 = CARTESIAN_POINT ( 'NONE',  ( 51.09375000000000000, 11.65685424949236193, 10.99999999999998401 ) ) ;
#5219 = CARTESIAN_POINT ( 'NONE',  ( 1.432654583217642275, -3.458734124999999437, 3.050000001365598568 ) ) ;
#5220 = FILL_AREA_STYLE ('',( #21613 ) ) ;
#5221 = CARTESIAN_POINT ( 'NONE',  ( -3.458734124999998105, 1.432654583217640276, 16.37500000136560629 ) ) ;
#5222 = DIRECTION ( 'NONE',  ( 0.000000000000000000, 0.000000000000000000, 1.000000000000000000 ) ) ;
#5223 = EDGE_CURVE ( 'NONE', #1016, #16967, #15690, .T. ) ;
#5224 = DIRECTION ( 'NONE',  ( -0.000000000000000000, -0.000000000000000000, 1.000000000000000000 ) ) ;
#5225 = ORIENTED_EDGE ( 'NONE', *, *, #23090, .F. ) ;
#5226 = CARTESIAN_POINT ( 'NONE',  ( -3.394711121928224884, -0.8419189903391639529, 2.040000000000001368 ) ) ;
#5227 = EDGE_CURVE ( 'NONE', #5741, #946, #12107, .T. ) ;
#5228 = CARTESIAN_POINT ( 'NONE',  ( -31.74999999999995737, 0.000000000000000000, 2.500000000000000444 ) ) ;
#5229 = CARTESIAN_POINT ( 'NONE',  ( -1.600000000000004086, 0.000000000000000000, 0.000000000000000000 ) ) ;
#5230 = VERTEX_POINT ( 'NONE', #4644 ) ;
#5231 = LINE ( 'NONE', #17934, #8332 ) ;
#5232 = ADVANCED_FACE ( 'NONE', ( #11978 ), #2833, .T. ) ;
#5233 = CARTESIAN_POINT ( 'NONE',  ( 67.29999999999999716, 9.999999999999998224, 12.49999999999999289 ) ) ;
#5234 = VERTEX_POINT ( 'NONE', #1748 ) ;
#5235 = CARTESIAN_POINT ( 'NONE',  ( -68.40000000218495302, 12.50000000000000000, 14.99999999999999645 ) ) ;
#5236 = ORIENTED_EDGE ( 'NONE', *, *, #21069, .T. ) ;
#5237 = AXIS2_PLACEMENT_3D ( 'NONE', #7022, #19817, #12429 ) ;
#5238 = CARTESIAN_POINT ( 'NONE',  ( 52.96875000000000000, 5.999999999999987566, 13.34314575050763452 ) ) ;
#5239 = CARTESIAN_POINT ( 'NONE',  ( 67.65000000218496723, 12.50000000000000000, 16.03553390593273420 ) ) ;
#5240 = CIRCLE ( 'NONE', #15607, 11.00000000000000000 ) ;
#5241 = DIRECTION ( 'NONE',  ( 0.000000000000000000, 0.000000000000000000, 1.000000000000000000 ) ) ;
#5242 = CARTESIAN_POINT ( 'NONE',  ( -68.74999999999998579, 7.499999999999996447, 13.96446609406725514 ) ) ;
#5243 = PLANE ( 'NONE',  #5691 ) ;
#5244 = ORIENTED_EDGE ( 'NONE', *, *, #22032, .T. ) ;
#5245 = CARTESIAN_POINT ( 'NONE',  ( 9.920644283265380691E-16, 4.000000000000000000, 17.87500000273119483 ) ) ;
#5246 = MECHANICAL_DESIGN_GEOMETRIC_PRESENTATION_REPRESENTATION (  '', ( #2178 ), #23613 ) ;
#5247 = DIRECTION ( 'NONE',  ( 0.000000000000000000, 0.000000000000000000, -1.000000000000000000 ) ) ;
#5248 = CARTESIAN_POINT ( 'NONE',  ( 58.84143183416158962, 8.275094609562001935, 18.97181229448536044 ) ) ;
#5249 = DIRECTION ( 'NONE',  ( 1.000000000000000000, 3.273063162220391312E-16, 0.000000000000000000 ) ) ;
#5250 = CARTESIAN_POINT ( 'NONE',  ( 67.85000000109246798, 9.999999999999998224, 12.93301269999999192 ) ) ;
#5251 = VECTOR ( 'NONE', #11361, 1000.000000000000114 ) ;
#5252 = DIRECTION ( 'NONE',  ( -0.3420201433256622181, 0.9396926207859106484, 1.232595164407828100E-31 ) ) ;
#5253 = AXIS2_PLACEMENT_3D ( 'NONE', #10069, #20693, #18794 ) ;
#5254 = ADVANCED_FACE ( 'NONE', ( #12444, #19594 ), #1382, .F. ) ;
#5255 = CARTESIAN_POINT ( 'NONE',  ( 44.00000000000000711, -9.000000000000003553, 11.00000000000008882 ) ) ;
#5256 = ORIENTED_EDGE ( 'NONE', *, *, #18296, .T. ) ;
#5257 = CARTESIAN_POINT ( 'NONE',  ( 72.50000000000000000, 9.999999999999998224, 14.99999999999999645 ) ) ;
#5258 = EDGE_CURVE ( 'NONE', #2469, #1543, #6683, .T. ) ;
#5259 = CARTESIAN_POINT ( 'NONE',  ( 55.50000000000000711, 12.12132034355963484, 12.87867965644034740 ) ) ;
#5260 =( NAMED_UNIT ( * ) SI_UNIT ( $, .STERADIAN. ) SOLID_ANGLE_UNIT ( ) );
#5261 = ORIENTED_EDGE ( 'NONE', *, *, #18561, .F. ) ;
#5262 = DIRECTION ( 'NONE',  ( 7.087422195345011518E-32, 1.000000000000000000, -0.000000000000000000 ) ) ;
#5263 = VECTOR ( 'NONE', #10497, 1000.000000000000000 ) ;
#5264 = CARTESIAN_POINT ( 'NONE',  ( -1.432654583217640276, 3.458734125000000326, -1.449999998634403653 ) ) ;
#5265 = CARTESIAN_POINT ( 'NONE',  ( -65.90000000109246514, 9.143825827087049163, 17.06698729999999742 ) ) ;
#5266 = EDGE_CURVE ( 'NONE', #10129, #18029, #11343, .T. ) ;
#5267 = VERTEX_POINT ( 'NONE', #5112 ) ;
#5268 = FACE_OUTER_BOUND ( 'NONE', #13397, .T. ) ;
#5269 = ORIENTED_EDGE ( 'NONE', *, *, #4103, .F. ) ;
#5270 = ADVANCED_FACE ( 'NONE', ( #23317 ), #12696, .F. ) ;
#5271 = CIRCLE ( 'NONE', #18649, 4.000000000000000888 ) ;
#5272 = CARTESIAN_POINT ( 'NONE',  ( 4.000000000000000888, 4.898587196589412829E-16, 12.62500000273119660 ) ) ;
#5273 = CARTESIAN_POINT ( 'NONE',  ( -3.999999999999999112, 0.000000000000000000, 19.00000000000001066 ) ) ;
#5274 = FACE_OUTER_BOUND ( 'NONE', #14776, .T. ) ;
#5275 = AXIS2_PLACEMENT_3D ( 'NONE', #16971, #7872, #15193 ) ;
#5276 = DIRECTION ( 'NONE',  ( -0.000000000000000000, -0.000000000000000000, 1.000000000000000000 ) ) ;
#5277 = SURFACE_STYLE_USAGE ( .BOTH. , #7086 ) ;
#5278 = DIRECTION ( 'NONE',  ( 1.224646799147353207E-16, -0.000000000000000000, 1.000000000000000000 ) ) ;
#5279 = CARTESIAN_POINT ( 'NONE',  ( -67.04999999999999716, 7.499999999999995559, 16.03553390593273420 ) ) ;
#5280 = DIRECTION ( 'NONE',  ( 0.000000000000000000, 0.000000000000000000, -1.000000000000000000 ) ) ;
#5281 = CARTESIAN_POINT ( 'NONE',  ( 0.000000000000000000, 3.174628368996190719, -8.152713396088728359 ) ) ;
#5282 = CARTESIAN_POINT ( 'NONE',  ( 4.211140560182196957, -2.431303136016555122, -3.745885042887436622 ) ) ;
#5283 = AXIS2_PLACEMENT_3D ( 'NONE', #5400, #10929, #14643 ) ;
#5284 = CARTESIAN_POINT ( 'NONE',  ( 2.828427124746189847, 2.828427124746190291, 4.925000000000000711 ) ) ;
#5285 = CARTESIAN_POINT ( 'NONE',  ( -66.75000000109245946, 8.538419263543522320, 16.46158073645647235 ) ) ;
#5286 = EDGE_CURVE ( 'NONE', #735, #19572, #23004, .T. ) ;
#5287 = CARTESIAN_POINT ( 'NONE',  ( 68.60000000218495586, 9.999999999999998224, 17.49999999999999645 ) ) ;
#5288 = CARTESIAN_POINT ( 'NONE',  ( 1.025207404391860050E-15, 3.458734125000000326, 17.18750000136560274 ) ) ;
#5289 = CARTESIAN_POINT ( 'NONE',  ( 4.999999999999999112, -9.314797388894900720, 1.239665997526853580 ) ) ;
#5290 = AXIS2_PLACEMENT_3D ( 'NONE', #7616, #21845, #9300 ) ;
#5291 = ORIENTED_EDGE ( 'NONE', *, *, #6200, .T. ) ;
#5292 = VECTOR ( 'NONE', #18609, 1000.000000000000000 ) ;
#5293 = CARTESIAN_POINT ( 'NONE',  ( -71.55000000109247082, 8.538419263543524096, 13.53841926354352054 ) ) ;
#5294 = ORIENTED_EDGE ( 'NONE', *, *, #11158, .F. ) ;
#5295 = CARTESIAN_POINT ( 'NONE',  ( 54.71643183416158251, 13.97181229448536399, 16.72490539043799629 ) ) ;
#5296 = CARTESIAN_POINT ( 'NONE',  ( -66.60000000109248219, 7.933012699999995476, 15.85617417291294196 ) ) ;
#5297 = DIRECTION ( 'NONE',  ( 0.9999999999999998890, -1.232595164407830809E-32, 1.717409762921616818E-48 ) ) ;
#5298 = EDGE_CURVE ( 'NONE', #10244, #22841, #8853, .T. ) ;
#5299 = CARTESIAN_POINT ( 'NONE',  ( 6.353591512924457348E-16, -3.458734125000000326, -3.012499998634404541 ) ) ;
#5300 = ORIENTED_EDGE ( 'NONE', *, *, #22976, .F. ) ;
#5301 = CARTESIAN_POINT ( 'NONE',  ( 27.50000000000000000, 4.500000000000006217, -33.66025403784446723 ) ) ;
#5302 = EDGE_CURVE ( 'NONE', #7612, #7146, #3549, .T. ) ;
#5303 = VERTEX_POINT ( 'NONE', #8974 ) ;
#5304 = CARTESIAN_POINT ( 'NONE',  ( -6.473970235329672780E-16, -4.862606272033106691, -3.745885042887442395 ) ) ;
#5305 = CARTESIAN_POINT ( 'NONE',  ( 52.34606816583843880, 8.825410453826357582, 18.02818770551464667 ) ) ;
#5306 = CIRCLE ( 'NONE', #8384, 5.000000000000000888 ) ;
#5307 = CARTESIAN_POINT ( 'NONE',  ( -70.35000000109248219, 11.46158073645647235, 16.46158073645647235 ) ) ;
#5308 = CARTESIAN_POINT ( 'NONE',  ( -69.10000000109246798, 9.143825827087049163, 17.06698729999999742 ) ) ;
#5309 = CIRCLE ( 'NONE', #8388, 8.239200000000002078 ) ;
#5310 = CARTESIAN_POINT ( 'NONE',  ( -1.432654583217639832, -3.458734125000000326, 14.87500000136560807 ) ) ;
#5311 = CARTESIAN_POINT ( 'NONE',  ( -1.656854249492380138, -3.999999999999999112, 11.31250000273119660 ) ) ;
#5312 = CARTESIAN_POINT ( 'NONE',  ( 53.53125000000000000, 11.24264068711929276, 18.00000000000000355 ) ) ;
#5313 = CARTESIAN_POINT ( 'NONE',  ( 67.04999999999999716, 7.499999999999996447, 16.03553390593273775 ) ) ;
#5314 = CARTESIAN_POINT ( 'NONE',  ( 58.31250000000000000, 13.00000000000000000, 14.99999999999998757 ) ) ;
#5315 = CARTESIAN_POINT ( 'NONE',  ( 3.458734125000000770, 1.432654583217640498, -2.449999998634404097 ) ) ;
#5316 = CARTESIAN_POINT ( 'NONE',  ( -3.999999999999999112, 0.000000000000000000, 19.12500000273119838 ) ) ;
#5317 = AXIS2_PLACEMENT_3D ( 'NONE', #15592, #2621, #15237 ) ;
#5318 = LINE ( 'NONE', #3520, #17966 ) ;
#5319 = VECTOR ( 'NONE', #2740, 1000.000000000000000 ) ;
#5320 = EDGE_LOOP ( 'NONE', ( #11870, #15254, #9492, #14750 ) ) ;
#5321 = FACE_OUTER_BOUND ( 'NONE', #604, .T. ) ;
#5322 = CARTESIAN_POINT ( 'NONE',  ( 4.999999999999999112, -9.241976615262146311, 2.300561732649528679 ) ) ;
#5323 = ORIENTED_EDGE ( 'NONE', *, *, #3924, .T. ) ;
#5324 = CARTESIAN_POINT ( 'NONE',  ( 55.78125000000000000, 8.757359312880703683, 11.99999999999999822 ) ) ;
#5325 = CARTESIAN_POINT ( 'NONE',  ( 2.828427124746189847, 2.828427124746190291, 1.050000002731187321 ) ) ;
#5326 = EDGE_CURVE ( 'NONE', #21232, #11906, #8319, .T. ) ;
#5327 = CARTESIAN_POINT ( 'NONE',  ( 4.332341089154587834E-16, 7.505553499465137612, -3.700000000000000178 ) ) ;
#5328 = EDGE_LOOP ( 'NONE', ( #5201, #3265, #1751, #7163 ) ) ;
#5329 = CARTESIAN_POINT ( 'NONE',  ( 2.828427124746191179, 2.828427124746190291, 16.62500000000001066 ) ) ;
#5330 = ORIENTED_EDGE ( 'NONE', *, *, #13776, .F. ) ;
#5331 = CIRCLE ( 'NONE', #23687, 11.00000000000000000 ) ;
#5332 = DIRECTION ( 'NONE',  ( -7.087422195345011518E-32, -1.000000000000000000, -0.000000000000000000 ) ) ;
#5333 = COLOUR_RGB ( '', 0.66274510, 0.83137255, 0.94901961) ;
#5334 = CARTESIAN_POINT ( 'NONE',  ( -1.656854249492380582, 4.000000000000000000, -2.762499997268812457 ) ) ;
#5335 = VERTEX_POINT ( 'NONE', #17931 ) ;
#5336 = DIRECTION ( 'NONE',  ( 1.224646799147353207E-16, -0.000000000000000000, 1.000000000000000000 ) ) ;
#5337 = DIRECTION ( 'NONE',  ( 1.000000000000000000, 0.000000000000000000, 0.000000000000000000 ) ) ;
#5338 = EDGE_LOOP ( 'NONE', ( #11683, #5436, #21600, #13629, #12518 ) ) ;
#5339 = CIRCLE ( 'NONE', #16443, 4.999999999999999112 ) ;
#5340 = CARTESIAN_POINT ( 'NONE',  ( -60.00000000000000711, -15.00000000000000000, 20.00000000000001421 ) ) ;
#5341 = CARTESIAN_POINT ( 'NONE',  ( 70.50000000000000000, 9.999999999999998224, 12.49999999999999289 ) ) ;
#5342 = DIRECTION ( 'NONE',  ( 0.000000000000000000, -0.8090169943749530024, 0.5877852522924653655 ) ) ;
#5343 = PLANE ( 'NONE',  #1118 ) ;
#5344 = CARTESIAN_POINT ( 'NONE',  ( 58.06481816583843170, 5.999999999999996447, 15.06805114094564502 ) ) ;
#5345 = CARTESIAN_POINT ( 'NONE',  ( 3.458734125000000326, 1.432654583217640498, -0.6999999986344048741 ) ) ;
#5346 = PRESENTATION_STYLE_ASSIGNMENT (( #1740 ) ) ;
#5347 = CARTESIAN_POINT ( 'NONE',  ( -1.301042606982605321E-15, 7.505553499465137612, -0.5805565836007695601 ) ) ;
#5348 = CARTESIAN_POINT ( 'NONE',  ( -19.99999999999999645, -9.000000000000003553, 5.000000000000079936 ) ) ;
#5349 = CARTESIAN_POINT ( 'NONE',  ( 50.00000000000000000, -7.098169556225942145, 56.71010071662853136 ) ) ;
#5350 = ORIENTED_EDGE ( 'NONE', *, *, #9801, .T. ) ;
#5351 = LINE ( 'NONE', #9314, #15340 ) ;
#5352 = CARTESIAN_POINT ( 'NONE',  ( 68.34999999999999432, 12.50000000000000000, 16.03553390593273775 ) ) ;
#5353 = CARTESIAN_POINT ( 'NONE',  ( 50.00000000000000711, -10.03966385473555789, 5.000000000000079936 ) ) ;
#5354 = VERTEX_POINT ( 'NONE', #21741 ) ;
#5355 = AXIS2_PLACEMENT_3D ( 'NONE', #22100, #2107, #20309 ) ;
#5356 = EDGE_LOOP ( 'NONE', ( #12306, #7138, #18058, #20002 ) ) ;
#5357 = VECTOR ( 'NONE', #22801, 1000.000000000000000 ) ;
#5358 = CARTESIAN_POINT ( 'NONE',  ( -1.656854249492379472, 4.000000000000000000, 13.93750000273119483 ) ) ;
#5359 = CARTESIAN_POINT ( 'NONE',  ( 56.71875000000000711, 14.00000000000001066, 16.65685424949235482 ) ) ;
#5360 = ORIENTED_EDGE ( 'NONE', *, *, #9865, .T. ) ;
#5361 = DIRECTION ( 'NONE',  ( -1.000000000000000000, -0.000000000000000000, -0.000000000000000000 ) ) ;
#5362 = VERTEX_POINT ( 'NONE', #10884 ) ;
#5363 = CARTESIAN_POINT ( 'NONE',  ( 52.12500000000000711, 12.82842712474620228, 17.82842712474617386 ) ) ;
#5364 = CONICAL_SURFACE ( 'NONE', #777, 2.041999999999999815, 1.047197551196591858 ) ;
#5365 = CARTESIAN_POINT ( 'NONE',  ( 66.90000000218495302, 11.76776695296636888, 16.76776695296636532 ) ) ;
#5366 = EDGE_CURVE ( 'NONE', #22997, #13902, #4040, .T. ) ;
#5367 = FACE_OUTER_BOUND ( 'NONE', #21920, .T. ) ;
#5368 = DIRECTION ( 'NONE',  ( 0.000000000000000000, 0.000000000000000000, 1.000000000000000000 ) ) ;
#5369 = CARTESIAN_POINT ( 'NONE',  ( 0.000000000000000000, 0.000000000000000000, 0.000000000000000000 ) ) ;
#5370 = ORIENTED_EDGE ( 'NONE', *, *, #14340, .T. ) ;
#5371 = CARTESIAN_POINT ( 'NONE',  ( 4.000000000000000888, 1.656854249492381248, 17.68750000273119483 ) ) ;
#5372 = CARTESIAN_POINT ( 'NONE',  ( 30.70991776966726405, -11.25000000000000355, 5.000000000000079936 ) ) ;
#5373 = CARTESIAN_POINT ( 'NONE',  ( 53.49768183416157541, 12.16943976678977535, 12.92679907967048614 ) ) ;
#5374 = CARTESIAN_POINT ( 'NONE',  ( -14.99999999999997335, -15.00000000000000000, -49.99999999999999289 ) ) ;
#5375 = EDGE_CURVE ( 'NONE', #18055, #15893, #13255, .T. ) ;
#5376 = CARTESIAN_POINT ( 'NONE',  ( 66.65000000109247935, 9.999999999999998224, 17.06698730000000097 ) ) ;
#5377 = CIRCLE ( 'NONE', #18768, 8.749000000000000554 ) ;
#5378 = CARTESIAN_POINT ( 'NONE',  ( -69.05000000000002558, 12.50000000000000000, 13.96446609406725692 ) ) ;
#5379 = DIRECTION ( 'NONE',  ( -1.000000000000000000, -0.000000000000000000, 0.000000000000000000 ) ) ;
#5380 = CIRCLE ( 'NONE', #18771, 4.000000000000002665 ) ;
#5381 = ORIENTED_EDGE ( 'NONE', *, *, #18595, .T. ) ;
#5382 = DIRECTION ( 'NONE',  ( 1.000000000000000000, -0.000000000000000000, 0.000000000000000000 ) ) ;
#5383 = CARTESIAN_POINT ( 'NONE',  ( 59.25000000000000711, 7.878679656440361612, 17.12132034355964549 ) ) ;
#5384 = DIRECTION ( 'NONE',  ( 0.000000000000000000, 0.000000000000000000, 1.000000000000000000 ) ) ;
#5385 = CARTESIAN_POINT ( 'NONE',  ( -72.25000000000000000, 12.50000000000000000, 13.96446609406725692 ) ) ;
#5386 = ORIENTED_EDGE ( 'NONE', *, *, #15305, .T. ) ;
#5387 = CYLINDRICAL_SURFACE ( 'NONE', #12458, 2.499999999999998668 ) ;
#5388 = CARTESIAN_POINT ( 'NONE',  ( 3.458734125000000770, -1.432654583217639610, -2.824999998634404985 ) ) ;
#5389 = DIRECTION ( 'NONE',  ( -1.000000000000000000, -0.000000000000000000, -0.000000000000000000 ) ) ;
#5390 = ORIENTED_EDGE ( 'NONE', *, *, #2492, .T. ) ;
#5391 = CARTESIAN_POINT ( 'NONE',  ( 4.000000000000000888, 4.898587196589412829E-16, 21.31370849898476649 ) ) ;
#5392 = ORIENTED_EDGE ( 'NONE', *, *, #845, .T. ) ;
#5393 = CARTESIAN_POINT ( 'NONE',  ( 2.828427124746191179, 2.828427124746190291, 18.62500000000001066 ) ) ;
#5394 = CARTESIAN_POINT ( 'NONE',  ( -3.458734124999999437, 0.000000000000000000, 10.68750000136560452 ) ) ;
#5395 = CARTESIAN_POINT ( 'NONE',  ( 2.499999999999999556, 5.222868219166995729, -9.680994141368717720 ) ) ;
#5396 = AXIS2_PLACEMENT_3D ( 'NONE', #15241, #17138, #2508 ) ;
#5397 = EDGE_CURVE ( 'NONE', #12965, #4570, #1629, .T. ) ;
#5398 = CARTESIAN_POINT ( 'NONE',  ( -67.80000000218494449, 9.999999999999998224, 17.49999999999999645 ) ) ;
#5399 = ADVANCED_FACE ( 'NONE', ( #15909, #23186 ), #16148, .T. ) ;
#5400 = CARTESIAN_POINT ( 'NONE',  ( -2.000000000000001776, 0.000000000000000000, 0.000000000000000000 ) ) ;
#5401 = CARTESIAN_POINT ( 'NONE',  ( 0.000000000000000000, -9.241976615262146311, -1.699438267350473097 ) ) ;
#5402 = CARTESIAN_POINT ( 'NONE',  ( -66.49999999999998579, 9.999999999999998224, 12.49999999999999289 ) ) ;
#5403 = DIRECTION ( 'NONE',  ( -1.000000000000000000, -0.000000000000000000, -0.000000000000000000 ) ) ;
#5404 = EDGE_CURVE ( 'NONE', #7665, #13106, #12334, .T. ) ;
#5405 = CARTESIAN_POINT ( 'NONE',  ( -2.445694354108819191, 2.445694354108820523, 19.31250000136560629 ) ) ;
#5406 = CARTESIAN_POINT ( 'NONE',  ( 4.999999999999999112, 0.000000000000000000, 0.000000000000000000 ) ) ;
#5407 = CARTESIAN_POINT ( 'NONE',  ( 4.000000000000000888, -1.656854249492379694, 4.737499999999999822 ) ) ;
#5408 = PLANE ( 'NONE',  #19136 ) ;
#5409 = CARTESIAN_POINT ( 'NONE',  ( -3.458734124999998993, 0.000000000000000000, 19.43750000136560629 ) ) ;
#5410 = DIRECTION ( 'NONE',  ( 1.000000000000000000, -0.000000000000000000, -0.000000000000000000 ) ) ;
#5411 = EDGE_LOOP ( 'NONE', ( #22059, #11337, #6010, #243 ) ) ;
#5412 = CARTESIAN_POINT ( 'NONE',  ( -69.00000000109247367, 7.933012699999995476, 15.85617417291294196 ) ) ;
#5413 = ORIENTED_EDGE ( 'NONE', *, *, #19192, .F. ) ;
#5414 = CARTESIAN_POINT ( 'NONE',  ( 52.56018183416157541, 5.999999999999996447, 14.93194885905437808 ) ) ;
#5415 = CARTESIAN_POINT ( 'NONE',  ( -68.05000000109247082, 9.999999999999998224, 17.06698730000000097 ) ) ;
#5416 = DIRECTION ( 'NONE',  ( 1.000000000000000000, -6.123233995736766036E-17, -6.123233995736764803E-17 ) ) ;
#5417 = CARTESIAN_POINT ( 'NONE',  ( -2.449293598294706907E-16, 4.000000000000000000, 1.175000002731187543 ) ) ;
#5418 = ORIENTED_EDGE ( 'NONE', *, *, #9504, .F. ) ;
#5419 = EDGE_CURVE ( 'NONE', #22275, #16998, #4141, .T. ) ;
#5420 = ORIENTED_EDGE ( 'NONE', *, *, #4804, .T. ) ;
#5421 = CARTESIAN_POINT ( 'NONE',  ( 1.432654583217641386, 3.458734125000000770, 19.37500000136560274 ) ) ;
#5422 = CARTESIAN_POINT ( 'NONE',  ( 54.03356816583844591, 11.31069182806492712, 17.97181229448534623 ) ) ;
#5423 = B_SPLINE_CURVE_WITH_KNOTS ( 'NONE', 3,
 ( #22176, #2421, #4106, #5909, #16816, #5791 ),
 .UNSPECIFIED., .F., .F.,
 ( 4, 2, 4 ),
 ( -3.640115492407174633E-06, 0.0002066546034006553863, 0.0004169493222937179812 ),
 .UNSPECIFIED. ) ;
#5424 = CARTESIAN_POINT ( 'NONE',  ( -70.45000000109247651, 9.999999999999998224, 17.06698730000000097 ) ) ;
#5425 = ADVANCED_FACE ( 'NONE', ( #5821 ), #1859, .F. ) ;
#5426 = CARTESIAN_POINT ( 'NONE',  ( -69.85000000109246798, 9.999999999999998224, 17.06698730000000097 ) ) ;
#5427 = CARTESIAN_POINT ( 'NONE',  ( 1.025207404391860050E-15, 3.458734125000000770, 13.43750000136560452 ) ) ;
#5428 = CARTESIAN_POINT ( 'NONE',  ( 72.50000000000000000, 9.999999999999998224, 14.99999999999999645 ) ) ;
#5429 = ADVANCED_FACE ( 'NONE', ( #20534 ), #13269, .F. ) ;
#5430 = CARTESIAN_POINT ( 'NONE',  ( 51.37500000000000711, 7.878679656440349177, 12.87867965644035984 ) ) ;
#5431 = DIRECTION ( 'NONE',  ( 1.000000000000000000, 0.000000000000000000, 0.000000000000000000 ) ) ;
#5432 = ADVANCED_FACE ( 'NONE', ( #18758 ), #12922, .T. ) ;
#5433 = CARTESIAN_POINT ( 'NONE',  ( 55.50000000000000711, 12.12132034355963484, 12.87867965644034740 ) ) ;
#5434 = CARTESIAN_POINT ( 'NONE',  ( -2.740672138314428796, -2.121953112084053128, 2.039999999999995595 ) ) ;
#5435 = PLANE ( 'NONE',  #20637 ) ;
#5436 = ORIENTED_EDGE ( 'NONE', *, *, #23158, .T. ) ;
#5437 = CARTESIAN_POINT ( 'NONE',  ( 69.80000000218494449, 9.999999999999998224, 12.49999999999999289 ) ) ;
#5438 = DIRECTION ( 'NONE',  ( 0.000000000000000000, 0.000000000000000000, -1.000000000000000000 ) ) ;
#5439 = EDGE_LOOP ( 'NONE', ( #22345, #22311, #2758, #21181 ) ) ;
#5440 = CARTESIAN_POINT ( 'NONE',  ( 52.21875000000002842, 13.00000000000000711, 16.24264068711927322 ) ) ;
#5441 =( NAMED_UNIT ( * ) PLANE_ANGLE_UNIT ( ) SI_UNIT ( $, .RADIAN. ) );
#5442 = CARTESIAN_POINT ( 'NONE',  ( -1.432654583217640276, 3.458734125000000326, 5.550000001365596347 ) ) ;
#5443 = AXIS2_PLACEMENT_3D ( 'NONE', #18536, #9458, #16756 ) ;
#5444 = CARTESIAN_POINT ( 'NONE',  ( -31.74999999999995737, 0.000000000000000000, 0.000000000000000000 ) ) ;
#5445 = ORIENTED_EDGE ( 'NONE', *, *, #17425, .T. ) ;
#5446 = CARTESIAN_POINT ( 'NONE',  ( -3.999999999999998224, -1.656854249492383246, 19.06250000000001421 ) ) ;
#5447 = CARTESIAN_POINT ( 'NONE',  ( -7.245101763170664455, -4.357596700699738257, 10.00000000000008882 ) ) ;
#5448 =( BOUNDED_CURVE ( )  B_SPLINE_CURVE ( 2, ( #13425, #11745, #921, #2251, #19010, #20690, #7786, #22244, #4294 ),
 .UNSPECIFIED., .F., .F. ) 
 B_SPLINE_CURVE_WITH_KNOTS ( ( 3, 2, 2, 2, 3 ),
 ( 0.3749999999999998890, 0.3906249999999997780, 0.4062499999999996669, 0.4218749999999996114, 0.4374999999999995004 ),
 .UNSPECIFIED. ) 
 CURVE ( )  GEOMETRIC_REPRESENTATION_ITEM ( )  RATIONAL_B_SPLINE_CURVE ( ( 1.000000000000000444, 0.9238795325112861834, 1.000000000000000000, 0.9238795325112867385, 1.000000000000000000, 0.9238795325112867385, 1.000000000000000000, 0.9238795325112891810, 0.9999999999999975575 ) ) 
 REPRESENTATION_ITEM ( '' )  );
#5449 = CARTESIAN_POINT ( 'NONE',  ( -10.00000000000000000, 0.000000000000000000, 0.000000000000000000 ) ) ;
#5450 = ORIENTED_EDGE ( 'NONE', *, *, #20433, .F. ) ;
#5451 = CARTESIAN_POINT ( 'NONE',  ( 2.499999999999999556, 1.464956435139696644, -10.90201369670497122 ) ) ;
#5452 = DIRECTION ( 'NONE',  ( 1.000000000000000000, -0.000000000000000000, 0.000000000000000000 ) ) ;
#5453 = CARTESIAN_POINT ( 'NONE',  ( 1.432654583217642053, -3.458734124999999882, 1.300000001365597013 ) ) ;
#5454 = CARTESIAN_POINT ( 'NONE',  ( 70.14999999999999147, 8.964466094067258695, 17.50000000000000355 ) ) ;
#5455 = EDGE_CURVE ( 'NONE', #20184, #11236, #4862, .T. ) ;
#5456 = CARTESIAN_POINT ( 'NONE',  ( -1.489200000000000301, 0.000000000000000000, -8.239200000000002078 ) ) ;
#5457 = EDGE_CURVE ( 'NONE', #19658, #9455, #18397, .T. ) ;
#5458 = CARTESIAN_POINT ( 'NONE',  ( 69.39999999999999147, 8.232233047033627571, 16.76776695296636532 ) ) ;
#5459 = CARTESIAN_POINT ( 'NONE',  ( 51.97106816583844591, 5.971812294485345340, 13.41119689145326710 ) ) ;
#5460 = CARTESIAN_POINT ( 'NONE',  ( 6.353591512924457348E-16, -3.458734125000000326, 0.9875000013655956810 ) ) ;
#5461 = SURFACE_SIDE_STYLE ('',( #3306 ) ) ;
#5462 = PLANE ( 'NONE',  #22364 ) ;
#5463 = CARTESIAN_POINT ( 'NONE',  ( 4.999999999999999112, 0.000000000000000000, 0.000000000000000000 ) ) ;
#5464 = VERTEX_POINT ( 'NONE', #22329 ) ;
#5465 = CARTESIAN_POINT ( 'NONE',  ( 6.500000000000000888, 0.000000000000000000, -3.700000000000000178 ) ) ;
#5466 = DIRECTION ( 'NONE',  ( -1.000000000000000000, 0.000000000000000000, 0.000000000000000000 ) ) ;
#5467 = CYLINDRICAL_SURFACE ( 'NONE', #173, 5.000000000000011546 ) ;
#5468 = ORIENTED_EDGE ( 'NONE', *, *, #23541, .T. ) ;
#5469 = VERTEX_POINT ( 'NONE', #9315 ) ;
#5470 = DIRECTION ( 'NONE',  ( -1.000000000000000000, 0.000000000000000000, -0.000000000000000000 ) ) ;
#5471 = CARTESIAN_POINT ( 'NONE',  ( 54.56250000000000711, 5.999999999999996447, 15.00000000000001599 ) ) ;
#5472 = ORIENTED_EDGE ( 'NONE', *, *, #4944, .T. ) ;
#5473 = CARTESIAN_POINT ( 'NONE',  ( -1.656854249492380138, -3.999999999999999112, 18.18750000000001066 ) ) ;
#5474 = ORIENTED_EDGE ( 'NONE', *, *, #17611, .F. ) ;
#5475 = AXIS2_PLACEMENT_3D ( 'NONE', #18191, #11149, #7068 ) ;
#5476 = CARTESIAN_POINT ( 'NONE',  ( 52.62731816583844591, 12.87654654797634102, 17.78030770151602979 ) ) ;
#5477 = AXIS2_PLACEMENT_3D ( 'NONE', #17290, #4582, #11795 ) ;
#5478 = CARTESIAN_POINT ( 'NONE',  ( 67.80000000218494449, 9.999999999999998224, 17.49999999999999645 ) ) ;
#5479 =( BOUNDED_SURFACE ( )  B_SPLINE_SURFACE ( 1, 2, ( 
 ( #4380, #22330, #17085, #11602, #18869, #11485, #4142, #18760, #16853, #2454, #13949, #15859, #18632, #2343, #431, #2218, #11358, #11717, #5944, #658, #9789, #7992, #9676, #16966, #543, #7756, #15314, #22586, #7867, #15189, #17655, #20535, #22449, #6062, #3014, #23133, #1215, #15073, #19418, #6189, #13510, #13395, #21205, #20662, #4267, #8121, #20774, #20413, #9559, #18983, #9915, #17212, #790, #15431, #23024, #4819, #6629, #12151, #10366, #6746, #4022, #21813, #10945, #1807, #12515, #14300, #23250, #10719, #19775, #21561, #1450, #4941, #12639, #1329, #12390, #8669, #22, #23379, #10835, #14053, #5415, #21685, #19543, #16092, #16326, #17761, #12752, #16206, #15967, #10603, #5057, #5174, #3379, #6859, #18109, #17877, #17996, #14547, #3138, #20004, #6982, #8787, #23492, #1573, #18224, #14184, #8911, #14422, #7105, #5296, #21444, #3606, #19655, #19898, #3500, #10480, #12277, #1689, #9154, #3256, #16440, #21321, #9033, #23617, #7231, #4085, #9380, #16793, #14660 ),
 ( #9626, #6008, #20117, #7817, #3720, #2288, #22156, #373, #7706, #245, #16917, #494, #20245, #18348, #18576, #15135, #14899, #15023, #22277, #7355, #1928, #18698, #9736, #5890, #21917, #13214, #2404, #22030, #11423, #20483, #14778, #22398, #13333, #20601, #4209, #11062, #11550, #9270, #5647, #18819, #17031, #16671, #3966, #16557, #5527, #12861, #133, #2157, #7462, #12981, #3852, #11187, #18461, #2042, #7580, #5775, #13102, #20358, #11302, #9494, #13684, #955, #21177, #22757, #13810, #17504, #19170, #20835, #10216, #2868, #6129, #11778, #18933, #2985, #9853, #20946, #21067, #2755, #4791, #2519, #6369, #13566, #15487, #840, #15252, #1073, #4443, #17150, #606, #728, #10339, #22519, #8289, #12127, #7932, #19391, #8061, #6489, #15375, #13458, #4324, #8174, #17273, #4564, #2638, #20720, #11900, #10095, #11665, #22642, #22875, #8415, #6246, #19047, #17386, #9982, #15608, #4678, #12012, #19277, #15728, #22998, #6604, #13922, #15939, #19628, #19868, #5265, #5145 ) ),
 .UNSPECIFIED., .F., .F., .F. ) 
 B_SPLINE_SURFACE_WITH_KNOTS ( ( 2, 2 ),
 ( 3, 2, 2, 2, 2, 2, 2, 2, 2, 2, 2, 2, 2, 2, 2, 2, 2, 2, 2, 2, 2, 2, 2, 2, 2, 2, 2, 2, 2, 2, 2, 2, 2, 2, 2, 2, 2, 2, 2, 2, 2, 2, 2, 2, 2, 2, 2, 2, 2, 2, 2, 2, 2, 2, 2, 2, 2, 2, 2, 2, 2, 2, 2, 2, 3 ),
 ( 0.000000000000000000, 1.000000000000000000 ),
 ( 0.000000000000000000, 0.01562500000000000000, 0.03125000000000000000, 0.04687500000000000000, 0.06250000000000000000, 0.07812500000000000000, 0.09375000000000000000, 0.1093750000000000000, 0.1250000000000000000, 0.1406250000000000000, 0.1562500000000000000, 0.1718750000000000000, 0.1875000000000000000, 0.2031250000000000000, 0.2187500000000000000, 0.2343750000000000000, 0.2500000000000000000, 0.2656250000000000000, 0.2812500000000000000, 0.2968750000000000000, 0.3125000000000000000, 0.3281250000000000000, 0.3437500000000000000, 0.3593750000000000000, 0.3750000000000000000, 0.3906250000000000000, 0.4062500000000000000, 0.4218750000000000000, 0.4375000000000000000, 0.4531250000000000000, 0.4687500000000000000, 0.4843750000000000000, 0.5000000000000000000, 0.5156250000000000000, 0.5312500000000000000, 0.5468750000000000000, 0.5625000000000000000, 0.5781250000000000000, 0.5937500000000000000, 0.6093750000000000000, 0.6250000000000000000, 0.6406250000000000000, 0.6562500000000000000, 0.6718750000000000000, 0.6875000000000000000, 0.7031250000000000000, 0.7187500000000000000, 0.7343750000000000000, 0.7500000000000000000, 0.7656250000000000000, 0.7812500000000000000, 0.7968750000000000000, 0.8125000000000000000, 0.8281250000000000000, 0.8437500000000000000, 0.8593750000000000000, 0.8750000000000000000, 0.8906250000000000000, 0.9062500000000000000, 0.9218750000000000000, 0.9375000000000000000, 0.9531250000000000000, 0.9687500000000000000, 0.9843750000000000000, 1.000000000000000000 ),
 .UNSPECIFIED. ) 
 GEOMETRIC_REPRESENTATION_ITEM ( )  RATIONAL_B_SPLINE_SURFACE ( (
 ( 1.000000000000000000, 0.9238795325112867385, 1.000000000000000000, 0.9238795325112867385, 1.000000000000000000, 0.9238795325112867385, 1.000000000000000000, 0.9238795325112867385, 1.000000000000000000, 0.9238795325112867385, 1.000000000000000000, 0.9238795325112867385, 1.000000000000000000, 0.9238795325112867385, 1.000000000000000000, 0.9238795325112867385, 1.000000000000000000, 0.9238795325112867385, 1.000000000000000000, 0.9238795325112867385, 1.000000000000000000, 0.9238795325112867385, 1.000000000000000000, 0.9238795325112867385, 1.000000000000000000, 0.9238795325112867385, 1.000000000000000000, 0.9238795325112867385, 1.000000000000000000, 0.9238795325112867385, 1.000000000000000000, 0.9238795325112867385, 1.000000000000000000, 0.9238795325112867385, 1.000000000000000000, 0.9238795325112867385, 1.000000000000000000, 0.9238795325112867385, 1.000000000000000000, 0.9238795325112867385, 1.000000000000000000, 0.9238795325112867385, 1.000000000000000000, 0.9238795325112867385, 1.000000000000000000, 0.9238795325112867385, 1.000000000000000000, 0.9238795325112867385, 1.000000000000000000, 0.9238795325112867385, 1.000000000000000000, 0.9238795325112867385, 1.000000000000000000, 0.9238795325112867385, 1.000000000000000000, 0.9238795325112867385, 1.000000000000000000, 0.9238795325112867385, 1.000000000000000000, 0.9238795325112867385, 1.000000000000000000, 0.9238795325112867385, 1.000000000000000000, 0.9238795325112867385, 1.000000000000000000, 0.9238795325112867385, 1.000000000000000000, 0.9238795325112867385, 1.000000000000000000, 0.9238795325112867385, 1.000000000000000000, 0.9238795325112867385, 1.000000000000000000, 0.9238795325112867385, 1.000000000000000000, 0.9238795325112867385, 1.000000000000000000, 0.9238795325112867385, 1.000000000000000000, 0.9238795325112867385, 1.000000000000000000, 0.9238795325112867385, 1.000000000000000000, 0.9238795325112867385, 1.000000000000000000, 0.9238795325112867385, 1.000000000000000000, 0.9238795325112867385, 1.000000000000000000, 0.9238795325112867385, 1.000000000000000000, 0.9238795325112867385, 1.000000000000000000, 0.9238795325112867385, 1.000000000000000000, 0.9238795325112867385, 1.000000000000000000, 0.9238795325112867385, 1.000000000000000000, 0.9238795325112867385, 1.000000000000000000, 0.9238795325112867385, 1.000000000000000000, 0.9238795325112867385, 1.000000000000000000, 0.9238795325112867385, 1.000000000000000000, 0.9238795325112867385, 1.000000000000000000, 0.9238795325112867385, 1.000000000000000000, 0.9238795325112867385, 1.000000000000000000, 0.9238795325112867385, 1.000000000000000000, 0.9238795325112867385, 1.000000000000000000, 0.9238795325112867385, 1.000000000000000000, 0.9238795325112867385, 1.000000000000000000, 0.9238795325112867385, 1.000000000000000000, 0.9238795325112867385, 1.000000000000000000, 0.9238795325112867385, 1.000000000000000000, 0.9238795325112867385, 1.000000000000000000),
 ( 1.000000000000000000, 0.9238795325112867385, 1.000000000000000000, 0.9238795325112867385, 1.000000000000000000, 0.9238795325112867385, 1.000000000000000000, 0.9238795325112867385, 1.000000000000000000, 0.9238795325112867385, 1.000000000000000000, 0.9238795325112867385, 1.000000000000000000, 0.9238795325112867385, 1.000000000000000000, 0.9238795325112867385, 1.000000000000000000, 0.9238795325112867385, 1.000000000000000000, 0.9238795325112867385, 1.000000000000000000, 0.9238795325112867385, 1.000000000000000000, 0.9238795325112867385, 1.000000000000000000, 0.9238795325112867385, 1.000000000000000000, 0.9238795325112867385, 1.000000000000000000, 0.9238795325112867385, 1.000000000000000000, 0.9238795325112867385, 1.000000000000000000, 0.9238795325112867385, 1.000000000000000000, 0.9238795325112867385, 1.000000000000000000, 0.9238795325112867385, 1.000000000000000000, 0.9238795325112867385, 1.000000000000000000, 0.9238795325112867385, 1.000000000000000000, 0.9238795325112867385, 1.000000000000000000, 0.9238795325112867385, 1.000000000000000000, 0.9238795325112867385, 1.000000000000000000, 0.9238795325112867385, 1.000000000000000000, 0.9238795325112867385, 1.000000000000000000, 0.9238795325112867385, 1.000000000000000000, 0.9238795325112867385, 1.000000000000000000, 0.9238795325112867385, 1.000000000000000000, 0.9238795325112867385, 1.000000000000000000, 0.9238795325112867385, 1.000000000000000000, 0.9238795325112867385, 1.000000000000000000, 0.9238795325112867385, 1.000000000000000000, 0.9238795325112867385, 1.000000000000000000, 0.9238795325112867385, 1.000000000000000000, 0.9238795325112867385, 1.000000000000000000, 0.9238795325112867385, 1.000000000000000000, 0.9238795325112867385, 1.000000000000000000, 0.9238795325112867385, 1.000000000000000000, 0.9238795325112867385, 1.000000000000000000, 0.9238795325112867385, 1.000000000000000000, 0.9238795325112867385, 1.000000000000000000, 0.9238795325112867385, 1.000000000000000000, 0.9238795325112867385, 1.000000000000000000, 0.9238795325112867385, 1.000000000000000000, 0.9238795325112867385, 1.000000000000000000, 0.9238795325112867385, 1.000000000000000000, 0.9238795325112867385, 1.000000000000000000, 0.9238795325112867385, 1.000000000000000000, 0.9238795325112867385, 1.000000000000000000, 0.9238795325112867385, 1.000000000000000000, 0.9238795325112867385, 1.000000000000000000, 0.9238795325112867385, 1.000000000000000000, 0.9238795325112867385, 1.000000000000000000, 0.9238795325112867385, 1.000000000000000000, 0.9238795325112867385, 1.000000000000000000, 0.9238795325112867385, 1.000000000000000000, 0.9238795325112867385, 1.000000000000000000, 0.9238795325112867385, 1.000000000000000000, 0.9238795325112867385, 1.000000000000000000, 0.9238795325112867385, 1.000000000000000000, 0.9238795325112867385, 1.000000000000000000, 0.9238795325112867385, 1.000000000000000000, 0.9238795325112867385, 1.000000000000000000) ) ) 
 REPRESENTATION_ITEM ( '' )  SURFACE ( )  );
#5480 = CARTESIAN_POINT ( 'NONE',  ( 41.56848460323381289, -9.000000000000001776, 10.00000000000008882 ) ) ;
#5481 = CARTESIAN_POINT ( 'NONE',  ( -19.99999999999999645, -9.000000000000003553, 5.000000000000079936 ) ) ;
#5482 = DIRECTION ( 'NONE',  ( 0.000000000000000000, 0.000000000000000000, 1.000000000000000000 ) ) ;
#5483 = ORIENTED_EDGE ( 'NONE', *, *, #22260, .T. ) ;
#5484 = CARTESIAN_POINT ( 'NONE',  ( 2.828427124746191179, 2.828427124746190291, 18.75000000273119483 ) ) ;
#5485 = LINE ( 'NONE', #16283, #16803 ) ;
#5486 = CARTESIAN_POINT ( 'NONE',  ( 54.34143183416158251, 8.275094609562001935, 18.97181229448536044 ) ) ;
#5487 = CARTESIAN_POINT ( 'NONE',  ( 3.194497824546384646, 2.392783823000994570, 2.039999999999998259 ) ) ;
#5488 = DIRECTION ( 'NONE',  ( 0.000000000000000000, 0.000000000000000000, -1.000000000000000000 ) ) ;
#5489 = FACE_OUTER_BOUND ( 'NONE', #1283, .T. ) ;
#5490 = CIRCLE ( 'NONE', #3573, 4.000000000000001776 ) ;
#5491 = CARTESIAN_POINT ( 'NONE',  ( 4.000000000000000000, 2.512223110932545023, -3.469391141908803711 ) ) ;
#5492 = VERTEX_POINT ( 'NONE', #7288 ) ;
#5493 = LINE ( 'NONE', #12721, #10105 ) ;
#5495 = VECTOR ( 'NONE', #18311, 1000.000000000000000 ) ;
#5494 = PRODUCT_RELATED_PRODUCT_CATEGORY ( 'part', '', ( #12046 ) ) ;
#5496 = CARTESIAN_POINT ( 'NONE',  ( 53.34375000000000000, 8.757359312880723223, 18.00000000000000711 ) ) ;
#5497 = DIRECTION ( 'NONE',  ( -1.000000000000000000, -0.000000000000000000, 0.000000000000000000 ) ) ;
#5498 = ORIENTED_EDGE ( 'NONE', *, *, #636, .F. ) ;
#5499 = EDGE_CURVE ( 'NONE', #20947, #3496, #16894, .T. ) ;
#5500 = CARTESIAN_POINT ( 'NONE',  ( -4.000000000000000000, -2.309401076758512694, -3.433295621305382461 ) ) ;
#5501 = CARTESIAN_POINT ( 'NONE',  ( -3.458734125000000326, 1.432654583217640276, -1.324999998634403653 ) ) ;
#5502 = DIRECTION ( 'NONE',  ( -0.000000000000000000, -0.000000000000000000, 1.000000000000000000 ) ) ;
#5503 = ORIENTED_EDGE ( 'NONE', *, *, #15949, .T. ) ;
#5504 = DIRECTION ( 'NONE',  ( 0.000000000000000000, 0.5877852522924688072, 0.8090169943749507819 ) ) ;
#5505 = VERTEX_POINT ( 'NONE', #21860 ) ;
#5506 = CARTESIAN_POINT ( 'NONE',  ( 1.656854249492381470, 4.000000000000000000, 18.81250000273119483 ) ) ;
#5507 = CARTESIAN_POINT ( 'NONE',  ( 1.656854249492381470, 4.000000000000000000, 16.68750000000001066 ) ) ;
#5508 = CARTESIAN_POINT ( 'NONE',  ( 4.999999999999999112, 10.90201369670498721, 1.464956435139581403 ) ) ;
#5509 = DIRECTION ( 'NONE',  ( 1.000000000000000000, 7.703719777548943412E-32, 0.000000000000000000 ) ) ;
#5510 =( LENGTH_UNIT ( ) NAMED_UNIT ( * ) SI_UNIT ( .MILLI., .METRE. ) );
#5511 = VERTEX_POINT ( 'NONE', #70 ) ;
#5512 = CARTESIAN_POINT ( 'NONE',  ( -68.34999999999999432, 12.50000000000000000, 16.03553390593273420 ) ) ;
#5513 = CARTESIAN_POINT ( 'NONE',  ( 60.00000000000000711, 12.82842712474617741, 12.17157287525379239 ) ) ;
#5514 = CARTESIAN_POINT ( 'NONE',  ( 66.30000000109247082, 12.06698730000000275, 15.85617417291294196 ) ) ;
#5515 = CARTESIAN_POINT ( 'NONE',  ( 3.458734125000001214, 1.432654583217640498, 16.00000000136560629 ) ) ;
#5516 = CARTESIAN_POINT ( 'NONE',  ( -3.264650091097280831E-13, -4.796980096169642493, -3.721999068284424617 ) ) ;
#5517 = CARTESIAN_POINT ( 'NONE',  ( -1.432654583217640498, 3.458734125000000770, -3.199999998634403209 ) ) ;
#5518 = CARTESIAN_POINT ( 'NONE',  ( 4.999999999999999112, -8.264486777890077462, -4.472189673936873611 ) ) ;
#5519 = CARTESIAN_POINT ( 'NONE',  ( -2.445694354108818303, -2.445694354108820523, 13.56250000136560629 ) ) ;
#5520 = DIRECTION ( 'NONE',  ( -1.000000000000000000, 0.000000000000000000, -0.000000000000000000 ) ) ;
#5521 = B_SPLINE_CURVE_WITH_KNOTS ( 'NONE', 3,
 ( #7950, #6150, #2771, #10112, #4339, #5047, #3003, #21193, #8898, #6619, #12380, #23480, #16194, #3364, #7094, #12625, #3488, #14172, #15955, #1205, #19645, #10354, #21551, #15849, #19887, #19405, #23237, #8657, #3246, #17751, #13937, #21433, #6847, #23014, #8542, #14290, #14411, #4807, #21307, #1435, #14042, #12139, #10592, #17863, #12505, #17644, #21672, #8776, #23121, #12266, #6734, #16081, #23368, #4929, #19762, #19531 ),
 .UNSPECIFIED., .F., .F.,
 ( 4, 2, 2, 2, 2, 2, 2, 2, 2, 2, 2, 2, 2, 2, 2, 2, 2, 2, 2, 2, 2, 2, 2, 2, 2, 2, 2, 4 ),
 ( 0.000000000000000000, 0.0009277918325622039331, 0.001855583665124407866, 0.002319479581405509399, 0.002783375497686610932, 0.003247271413967717235, 0.003711167330248823972, 0.004638959162811037013, 0.005566750995373249619, 0.006030646911654353320, 0.006262594869794909508, 0.006378568848865185867, 0.006494542827935463093, 0.006552529817470603875, 0.006610516807005745524, 0.006726490786076029689, 0.006958438744216604091, 0.007422334660497751160, 0.008350126493060048768, 0.009277918325622346377, 0.009741814241903491711, 0.01020571015818463531, 0.01113350199074691731, 0.01206129382330919410, 0.01298908565587147089, 0.01345298157215261102, 0.01391687748843375289, 0.01484466932099604008 ),
 .UNSPECIFIED. ) ;
#5522 = VERTEX_POINT ( 'NONE', #14599 ) ;
#5523 = EDGE_CURVE ( 'NONE', #7050, #22527, #16607, .T. ) ;
#5524 = CARTESIAN_POINT ( 'NONE',  ( -68.35000000109248219, 8.538419263543524096, 13.53841926354352054 ) ) ;
#5525 = VERTEX_POINT ( 'NONE', #5584 ) ;
#5526 = CARTESIAN_POINT ( 'NONE',  ( 58.09143183416158962, 11.72490539043799984, 11.02818770551463246 ) ) ;
#5527 = CARTESIAN_POINT ( 'NONE',  ( -70.05000000109247082, 7.933012699999995476, 14.99999999999999645 ) ) ;
#5528 = DIRECTION ( 'NONE',  ( 0.000000000000000000, 0.000000000000000000, 1.000000000000000000 ) ) ;
#5529 = EDGE_CURVE ( 'NONE', #2345, #19331, #20174, .T. ) ;
#5530 = CARTESIAN_POINT ( 'NONE',  ( -35.00000000000000711, 4.500000000000003553, -49.99999999999999289 ) ) ;
#5531 = ORIENTED_EDGE ( 'NONE', *, *, #12431, .T. ) ;
#5532 = ORIENTED_EDGE ( 'NONE', *, *, #3608, .T. ) ;
#5533 = CARTESIAN_POINT ( 'NONE',  ( 0.000000000000000000, 0.000000000000000000, 0.000000000000000000 ) ) ;
#5534 = ADVANCED_FACE ( 'NONE', ( #20412 ), #9432, .T. ) ;
#5535 = CARTESIAN_POINT ( 'NONE',  ( 52.53356816583844591, 11.31069182806492712, 17.97181229448534623 ) ) ;
#5536 = VECTOR ( 'NONE', #1664, 1000.000000000000000 ) ;
#5537 = AXIS2_PLACEMENT_3D ( 'NONE', #8226, #6421, #13737 ) ;
#5538 = CARTESIAN_POINT ( 'NONE',  ( -69.30000000109247082, 10.85617417291294551, 12.93301269999999370 ) ) ;
#5539 = CIRCLE ( 'NONE', #8616, 2.500000000000002220 ) ;
#5540 = CARTESIAN_POINT ( 'NONE',  ( -69.20000000109246230, 7.933012699999995476, 15.85617417291294196 ) ) ;
#5541 = CARTESIAN_POINT ( 'NONE',  ( 3.458734125000002546, -1.432654583217639610, 11.12500000136560452 ) ) ;
#5542 = LINE ( 'NONE', #5786, #9583 ) ;
#5543 = CARTESIAN_POINT ( 'NONE',  ( 51.93750000000000711, 10.00000000000000711, 17.99999999999999645 ) ) ;
#5544 = CARTESIAN_POINT ( 'NONE',  ( 71.79999999999998295, 8.232233047033627571, 16.76776695296636532 ) ) ;
#5545 = CARTESIAN_POINT ( 'NONE',  ( 54.46875000000000000, 6.999999999999992895, 13.75735931288071967 ) ) ;
#5546 = ADVANCED_FACE ( 'NONE', ( #11233 ), #7403, .T. ) ;
#5547 = CARTESIAN_POINT ( 'NONE',  ( 9.920644283265380691E-16, 4.000000000000000000, 15.87500000273119660 ) ) ;
#5548 = PLANE ( 'NONE',  #8428 ) ;
#5549 = ORIENTED_EDGE ( 'NONE', *, *, #8261, .T. ) ;
#5550 = CARTESIAN_POINT ( 'NONE',  ( 69.90000000218495302, 11.76776695296636888, 13.23223304703362579 ) ) ;
#5551 = EDGE_CURVE ( 'NONE', #15377, #20516, #15215, .T. ) ;
#5552 = DIRECTION ( 'NONE',  ( -1.000000000000000000, -0.000000000000000000, -0.000000000000000000 ) ) ;
#5553 = ORIENTED_EDGE ( 'NONE', *, *, #9100, .F. ) ;
#5554 = CARTESIAN_POINT ( 'NONE',  ( 56.81250000000000000, 13.00000000000000000, 14.99999999999998757 ) ) ;
#5555 = AXIS2_PLACEMENT_3D ( 'NONE', #11519, #812, #2373 ) ;
#5556 = CARTESIAN_POINT ( 'NONE',  ( -2.828427124746189403, -2.828427124746190735, -2.449999997268812457 ) ) ;
#5557 = EDGE_CURVE ( 'NONE', #21366, #9385, #14960, .T. ) ;
#5558 = CIRCLE ( 'NONE', #9780, 4.000000000000002665 ) ;
#5559 = CARTESIAN_POINT ( 'NONE',  ( -3.250000000000003997, -5.629165124598848102, 1.734723475976807094E-15 ) ) ;
#5560 = ORIENTED_EDGE ( 'NONE', *, *, #14173, .T. ) ;
#5561 = CARTESIAN_POINT ( 'NONE',  ( 4.000000000000000888, 4.898587196589412829E-16, 15.50000000000001066 ) ) ;
#5562 = CARTESIAN_POINT ( 'NONE',  ( -4.000000000000000000, -1.656854249492383024, -2.637499999999998845 ) ) ;
#5563 = CARTESIAN_POINT ( 'NONE',  ( 1.656854249492380138, 4.000000000000000000, -2.887499997268812457 ) ) ;
#5564 = ORIENTED_EDGE ( 'NONE', *, *, #8393, .F. ) ;
#5565 = EDGE_CURVE ( 'NONE', #15405, #844, #11058, .T. ) ;
#5566 = DIRECTION ( 'NONE',  ( 0.000000000000000000, 0.000000000000000000, -1.000000000000000000 ) ) ;
#5567 = ADVANCED_FACE ( 'NONE', ( #15072 ), #16965, .T. ) ;
#5568 = CARTESIAN_POINT ( 'NONE',  ( 19.99999999999998934, 9.999999999999964473, -50.00000000000000000 ) ) ;
#5569 = CARTESIAN_POINT ( 'NONE',  ( 3.458734125000000770, 1.432654583217640498, -0.4499999986344046521 ) ) ;
#5570 = VECTOR ( 'NONE', #16943, 1000.000000000000000 ) ;
#5571 = CARTESIAN_POINT ( 'NONE',  ( 67.64999999999999147, 11.03553390593273598, 17.50000000000000355 ) ) ;
#5572 = VECTOR ( 'NONE', #8850, 1000.000000000000000 ) ;
#5573 = LINE ( 'NONE', #12900, #8569 ) ;
#5574 = CARTESIAN_POINT ( 'NONE',  ( -19.99999999999999645, -9.000000000000003553, 5.000000000000079936 ) ) ;
#5575 = CARTESIAN_POINT ( 'NONE',  ( 50.84606816583843880, 8.411196891453267099, 19.02818770551464667 ) ) ;
#5576 = CARTESIAN_POINT ( 'NONE',  ( 6.353591512924457348E-16, -3.458734125000000326, 1.987500001365596569 ) ) ;
#5577 = CARTESIAN_POINT ( 'NONE',  ( 2.445694354108821411, 2.445694354108820523, 17.31250000136560629 ) ) ;
#5578 = DIRECTION ( 'NONE',  ( 1.000000000000000000, -0.000000000000000000, -0.000000000000000000 ) ) ;
#5579 = AXIS2_PLACEMENT_3D ( 'NONE', #17109, #10181, #1155 ) ;
#5580 = LINE ( 'NONE', #11230, #1352 ) ;
#5581 = EDGE_LOOP ( 'NONE', ( #11162, #14360, #3746, #3521 ) ) ;
#5582 = DIRECTION ( 'NONE',  ( 1.000000000000000000, 0.000000000000000000, -0.000000000000000000 ) ) ;
#5583 =( BOUNDED_SURFACE ( )  B_SPLINE_SURFACE ( 3, 2, ( 
 ( #4503, #10048, #17336 ),
 ( #11723, #8127, #9567 ),
 ( #4273, #8239, #18876 ),
 ( #5830, #7762, #17219 ),
 ( #15437, #2460, #550 ),
 ( #22592, #7999, #13630 ) ),
 .UNSPECIFIED., .F., .F., .F. ) 
 B_SPLINE_SURFACE_WITH_KNOTS ( ( 4, 2, 4 ),
 ( 3, 3 ),
 ( 0.02032853247518126918, 0.02278863295364821906, 0.02524873343211517240 ),
 ( 0.000000000000000000, 1.000000000000000000 ),
 .UNSPECIFIED. ) 
 GEOMETRIC_REPRESENTATION_ITEM ( )  RATIONAL_B_SPLINE_SURFACE ( (
 ( 1.000000000000000000, 0.8047781615896837382, 1.000000000000000000),
 ( 1.000000000000000000, 0.8123767586289252218, 1.000000000000000000),
 ( 1.000000000000000000, 0.8190662415564388121, 1.000000000000000000),
 ( 1.000000000000000000, 0.8192361015669026303, 1.000000000000000000),
 ( 1.000000000000000000, 0.8126135807103900266, 1.000000000000000000),
 ( 1.000000000000000000, 0.8047712338318593339, 1.000000000000000000) ) ) 
 REPRESENTATION_ITEM ( '' )  SURFACE ( )  );
#5584 = CARTESIAN_POINT ( 'NONE',  ( -20.00005079999999680, 3.872983346207417021, -1.000000000000000000 ) ) ;
#5585 = EDGE_CURVE ( 'NONE', #19783, #12772, #1014, .T. ) ;
#5586 = LINE ( 'NONE', #1749, #10548 ) ;
#5587 = ORIENTED_EDGE ( 'NONE', *, *, #5158, .F. ) ;
#5588 = ORIENTED_EDGE ( 'NONE', *, *, #17587, .T. ) ;
#5589 = DIRECTION ( 'NONE',  ( -1.000000000000000000, 0.000000000000000000, 1.224646799147353207E-16 ) ) ;
#5590 = EDGE_CURVE ( 'NONE', #701, #9988, #1078, .T. ) ;
#5591 = ORIENTED_EDGE ( 'NONE', *, *, #12863, .T. ) ;
#5592 = CARTESIAN_POINT ( 'NONE',  ( 56.43750000000000000, 10.00000000000001776, 18.99999999999999645 ) ) ;
#5593 = ORIENTED_EDGE ( 'NONE', *, *, #18616, .F. ) ;
#5594 = CARTESIAN_POINT ( 'NONE',  ( -1.800000000000000711, 0.000000000000000000, 0.000000000000000000 ) ) ;
#5595 = ORIENTED_EDGE ( 'NONE', *, *, #23008, .F. ) ;
#5596 = ADVANCED_FACE ( 'NONE', ( #2813 ), #22066, .F. ) ;
#5597 = B_SPLINE_CURVE_WITH_KNOTS ( 'NONE', 3,
 ( #23120, #19530, #3127, #10469, #6846, #21549 ),
 .UNSPECIFIED., .F., .F.,
 ( 4, 2, 4 ),
 ( 0.002365888236228001588, 0.003551327329835089319, 0.004736766423442177049 ),
 .UNSPECIFIED. ) ;
#5598 = CARTESIAN_POINT ( 'NONE',  ( 51.68981816583844591, 9.931948859054346102, 10.99999999999999467 ) ) ;
#5599 = CARTESIAN_POINT ( 'NONE',  ( 71.45000000109247651, 7.933012699999995476, 14.99999999999999645 ) ) ;
#5600 = CARTESIAN_POINT ( 'NONE',  ( 0.000000000000000000, 0.000000000000000000, 0.000000000000000000 ) ) ;
#5601 = CARTESIAN_POINT ( 'NONE',  ( 72.25000000109247367, 9.999999999999998224, 17.06698730000000097 ) ) ;
#5602 = CARTESIAN_POINT ( 'NONE',  ( -4.623144047065556705, -4.836380039389426955, -3.593844378834464059 ) ) ;
#5603 = ORIENTED_EDGE ( 'NONE', *, *, #17224, .T. ) ;
#5604 = CARTESIAN_POINT ( 'NONE',  ( 1.971781867644420635E-15, -4.000000000000000000, 16.37500000273119838 ) ) ;
#5605 = CARTESIAN_POINT ( 'NONE',  ( -1.393927851585477606, 4.043713361053528743, -3.526374918436835149 ) ) ;
#5606 = CARTESIAN_POINT ( 'NONE',  ( 54.62268183416157541, 12.78030770151606177, 17.87654654797631792 ) ) ;
#5607 = CARTESIAN_POINT ( 'NONE',  ( 1.065083781909167193, -6.890627091270381754, -3.442152416367922463 ) ) ;
#5608 = CARTESIAN_POINT ( 'NONE',  ( 66.85000000218495586, 12.50000000000000000, 16.03553390593273775 ) ) ;
#5609 = CARTESIAN_POINT ( 'NONE',  ( 72.50000000000000000, 9.999999999999998224, 14.99999999999999645 ) ) ;
#5610 = CARTESIAN_POINT ( 'NONE',  ( 4.211399257449709665, -2.459727064652517114, -3.751161691472417736 ) ) ;
#5611 = EDGE_LOOP ( 'NONE', ( #16531, #9922, #21319, #7484 ) ) ;
#5612 = CYLINDRICAL_SURFACE ( 'NONE', #5475, 4.000000000000000000 ) ;
#5613 = CARTESIAN_POINT ( 'NONE',  ( -4.000000000000000000, 1.677772373332757194, -3.535253723897187506 ) ) ;
#5614 = CARTESIAN_POINT ( 'NONE',  ( 18.96248019676620444, -9.000000000000005329, 10.00000000000008882 ) ) ;
#5615 = ORIENTED_EDGE ( 'NONE', *, *, #6110, .F. ) ;
#5616 = LINE ( 'NONE', #13650, #19307 ) ;
#5617 = CARTESIAN_POINT ( 'NONE',  ( -27.50000000000000711, 1.500000000000003109, -33.66025403784446723 ) ) ;
#5618 = CARTESIAN_POINT ( 'NONE',  ( 2.449848172108560096, 3.432307619358740514, -3.503702292528905637 ) ) ;
#5619 = ADVANCED_FACE ( 'NONE', ( #14515 ), #21779, .F. ) ;
#5620 = ORIENTED_EDGE ( 'NONE', *, *, #19578, .T. ) ;
#5621 = CARTESIAN_POINT ( 'NONE',  ( -4.000000000000000000, 0.000000000000000000, 1.300000000000000711 ) ) ;
#5622 = ORIENTED_EDGE ( 'NONE', *, *, #2592, .F. ) ;
#5623 =( BOUNDED_SURFACE ( )  B_SPLINE_SURFACE ( 1, 2, ( 
 ( #5316, #16340, #21581, #19799, #8688, #21707, #18129, #6766, #10746, #5195, #23512, #14082, #21345, #12535, #3397, #18019, #16226, #14439, #12658, #6027, #9285, #5792, #16817, #16691, #7371, #18720, #5666, #16573, #16461, #11080, #18836, #14680, #395, #13356, #2422, #4230, #18366, #22296, #152, #20623, #20133, #264, #9400, #13120, #18477, #21938, #22177, #7602, #40, #1947, #15039, #9644, #5547, #22048, #2181, #14799, #2058, #12880, #11325, #3985, #13236, #14922, #5910, #20264, #12998, #20379, #2311, #4107, #18598, #9520, #3869, #7726, #16935, #3741, #20502, #11447, #511, #7834, #15155, #22416, #11203, #11569, #7482, #17525, #17294, #19189, #2775, #9753, #4342, #21087, #12144, #976, #17051, #10115, #4813, #749, #13831, #17407, #17171, #8305, #10235, #12034, #8436, #22545, #1092, #6153, #8085, #15627, #19297, #11799, #6385, #20738, #22897, #4699, #19411, #20966, #2535, #6511, #626, #7954, #13941, #21199, #11681, #18950, #9876, #2661, #23018, #15395, #22775, #2888, #6623, #8193, #15747, #15274, #4585, #6268, #13476, #22658, #13585, #20852, #4459, #19071, #10003, #13703, #859, #11921, #15507, #4935, #8781 ),
 ( #5409, #17648, #3369, #23610, #12746, #14541, #21312, #8904, #3133, #7223, #6740, #3250, #19649, #23372, #5051, #1209, #16085, #10597, #10358, #12270, #1566, #19892, #8546, #8661, #12509, #1323, #12384, #15853, #21555, #14294, #23486, #17868, #16200, #6852, #15961, #1442, #5288, #14416, #5167, #6976, #23242, #19768, #3493, #23125, #10713, #17990, #7099, #21678, #12632, #10828, #14177, #18103, #1683, #9027, #16320, #21805, #3008, #14047, #19536, #10474, #17755, #21437, #3600, #20352, #15129, #11055, #367, #5769, #3713, #11294, #20473, #22271, #18691, #9147, #4079, #16434, #18342, #2151, #5883, #22025, #16664, #7347, #18568, #15017, #5999, #7573, #12854, #3960, #10939, #22390, #488, #7811, #14654, #21911, #5519, #12974, #9620, #20111, #9374, #9486, #16911, #18455, #16786, #13208, #14892, #16549, #11416, #2282, #1799, #7456, #1922, #19997, #9264, #238, #7700, #22150, #18218, #125, #2033, #14771, #11181, #20239, #16, #5640, #3846, #13096, #4202, #19041, #13560, #20595, #22512, #11895, #6483, #18813, #18927, #22752, #11657, #22636, #2397, #8168, #836, #10090, #6240, #2750, #17143, #2512, #15369, #15601, #950 ) ),
 .UNSPECIFIED., .F., .F., .F. ) 
 B_SPLINE_SURFACE_WITH_KNOTS ( ( 2, 2 ),
 ( 3, 2, 2, 2, 2, 2, 2, 2, 2, 2, 2, 2, 2, 2, 2, 2, 2, 2, 2, 2, 2, 2, 2, 2, 2, 2, 2, 2, 2, 2, 2, 2, 2, 2, 2, 2, 2, 2, 2, 2, 2, 2, 2, 2, 2, 2, 2, 2, 2, 2, 2, 2, 2, 2, 2, 2, 2, 2, 2, 2, 2, 2, 2, 2, 2, 2, 2, 2, 2, 2, 2, 2, 2, 2, 3 ),
 ( 0.000000000000000000, 1.000000000000000000 ),
 ( 0.000000000000000000, 0.01250000000000000069, 0.02500000000000000139, 0.03749999999999999861, 0.05000000000000000278, 0.06250000000000000000, 0.07499999999999999722, 0.08749999999999999445, 0.1000000000000000056, 0.1125000000000000028, 0.1250000000000000000, 0.1375000000000000111, 0.1499999999999999944, 0.1625000000000000056, 0.1749999999999999889, 0.1875000000000000000, 0.2000000000000000111, 0.2124999999999999944, 0.2250000000000000056, 0.2374999999999999889, 0.2500000000000000000, 0.2625000000000000111, 0.2750000000000000222, 0.2874999999999999778, 0.2999999999999999889, 0.3125000000000000000, 0.3250000000000000111, 0.3375000000000000222, 0.3499999999999999778, 0.3624999999999999889, 0.3750000000000000000, 0.3875000000000000111, 0.4000000000000000222, 0.4124999999999999778, 0.4249999999999999889, 0.4375000000000000000, 0.4500000000000000111, 0.4625000000000000222, 0.4749999999999999778, 0.4874999999999999889, 0.5000000000000000000, 0.5124999999999999556, 0.5250000000000000222, 0.5374999999999999778, 0.5500000000000000444, 0.5625000000000000000, 0.5749999999999999556, 0.5875000000000000222, 0.5999999999999999778, 0.6125000000000000444, 0.6250000000000000000, 0.6374999999999999556, 0.6500000000000000222, 0.6624999999999999778, 0.6750000000000000444, 0.6875000000000000000, 0.6999999999999999556, 0.7125000000000000222, 0.7249999999999999778, 0.7375000000000000444, 0.7500000000000000000, 0.7624999999999999556, 0.7750000000000000222, 0.7874999999999999778, 0.8000000000000000444, 0.8125000000000000000, 0.8249999999999999556, 0.8375000000000000222, 0.8499999999999999778, 0.8625000000000000444, 0.8750000000000000000, 0.8874999999999999556, 0.9000000000000000222, 0.9124999999999999778, 0.9250000000000000444 ),
 .UNSPECIFIED. ) 
 GEOMETRIC_REPRESENTATION_ITEM ( )  RATIONAL_B_SPLINE_SURFACE ( (
 ( 1.000000000000000000, 0.9238795325112867385, 1.000000000000000000, 0.9238795325112867385, 1.000000000000000000, 0.9238795325112867385, 1.000000000000000000, 0.9238795325112867385, 1.000000000000000000, 0.9238795325112867385, 1.000000000000000000, 0.9238795325112867385, 1.000000000000000000, 0.9238795325112867385, 1.000000000000000000, 0.9238795325112867385, 1.000000000000000000, 0.9238795325112867385, 1.000000000000000000, 0.9238795325112867385, 1.000000000000000000, 0.9238795325112867385, 1.000000000000000000, 0.9238795325112867385, 1.000000000000000000, 0.9238795325112867385, 1.000000000000000000, 0.9238795325112867385, 1.000000000000000000, 0.9238795325112867385, 1.000000000000000000, 0.9238795325112867385, 1.000000000000000000, 0.9238795325112867385, 1.000000000000000000, 0.9238795325112867385, 1.000000000000000000, 0.9238795325112867385, 1.000000000000000000, 0.9238795325112867385, 1.000000000000000000, 0.9238795325112867385, 1.000000000000000000, 0.9238795325112867385, 1.000000000000000000, 0.9238795325112867385, 1.000000000000000000, 0.9238795325112867385, 1.000000000000000000, 0.9238795325112867385, 1.000000000000000000, 0.9238795325112867385, 1.000000000000000000, 0.9238795325112867385, 1.000000000000000000, 0.9238795325112867385, 1.000000000000000000, 0.9238795325112867385, 1.000000000000000000, 0.9238795325112867385, 1.000000000000000000, 0.9238795325112867385, 1.000000000000000000, 0.9238795325112867385, 1.000000000000000000, 0.9238795325112867385, 1.000000000000000000, 0.9238795325112867385, 1.000000000000000000, 0.9238795325112867385, 1.000000000000000000, 0.9238795325112867385, 1.000000000000000000, 0.9238795325112867385, 1.000000000000000000, 0.9238795325112867385, 1.000000000000000000, 0.9238795325112867385, 1.000000000000000000, 0.9238795325112867385, 1.000000000000000000, 0.9238795325112867385, 1.000000000000000000, 0.9238795325112867385, 1.000000000000000000, 0.9238795325112867385, 1.000000000000000000, 0.9238795325112867385, 1.000000000000000000, 0.9238795325112867385, 1.000000000000000000, 0.9238795325112867385, 1.000000000000000000, 0.9238795325112867385, 1.000000000000000000, 0.9238795325112867385, 1.000000000000000000, 0.9238795325112867385, 1.000000000000000000, 0.9238795325112867385, 1.000000000000000000, 0.9238795325112867385, 1.000000000000000000, 0.9238795325112867385, 1.000000000000000000, 0.9238795325112867385, 1.000000000000000000, 0.9238795325112867385, 1.000000000000000000, 0.9238795325112867385, 1.000000000000000000, 0.9238795325112867385, 1.000000000000000000, 0.9238795325112867385, 1.000000000000000000, 0.9238795325112867385, 1.000000000000000000, 0.9238795325112867385, 1.000000000000000000, 0.9238795325112867385, 1.000000000000000000, 0.9238795325112867385, 1.000000000000000000, 0.9238795325112867385, 1.000000000000000000, 0.9238795325112867385, 1.000000000000000000, 0.9238795325112867385, 1.000000000000000000, 0.9238795325112867385, 1.000000000000000000, 0.9238795325112867385, 1.000000000000000000, 0.9238795325112867385, 1.000000000000000000, 0.9238795325112867385, 1.000000000000000000, 0.9238795325112867385, 1.000000000000000000, 0.9238795325112867385, 1.000000000000000000, 0.9238795325112867385, 1.000000000000000000, 0.9238795325112867385, 1.000000000000000000, 0.9238795325112867385, 1.000000000000000000, 0.9238795325112867385, 1.000000000000000000),
 ( 1.000000000000000000, 0.9238795325112867385, 1.000000000000000000, 0.9238795325112867385, 1.000000000000000000, 0.9238795325112867385, 1.000000000000000000, 0.9238795325112867385, 1.000000000000000000, 0.9238795325112867385, 1.000000000000000000, 0.9238795325112867385, 1.000000000000000000, 0.9238795325112867385, 1.000000000000000000, 0.9238795325112867385, 1.000000000000000000, 0.9238795325112867385, 1.000000000000000000, 0.9238795325112867385, 1.000000000000000000, 0.9238795325112867385, 1.000000000000000000, 0.9238795325112867385, 1.000000000000000000, 0.9238795325112867385, 1.000000000000000000, 0.9238795325112867385, 1.000000000000000000, 0.9238795325112867385, 1.000000000000000000, 0.9238795325112867385, 1.000000000000000000, 0.9238795325112867385, 1.000000000000000000, 0.9238795325112867385, 1.000000000000000000, 0.9238795325112867385, 1.000000000000000000, 0.9238795325112867385, 1.000000000000000000, 0.9238795325112867385, 1.000000000000000000, 0.9238795325112867385, 1.000000000000000000, 0.9238795325112867385, 1.000000000000000000, 0.9238795325112867385, 1.000000000000000000, 0.9238795325112867385, 1.000000000000000000, 0.9238795325112867385, 1.000000000000000000, 0.9238795325112867385, 1.000000000000000000, 0.9238795325112867385, 1.000000000000000000, 0.9238795325112867385, 1.000000000000000000, 0.9238795325112867385, 1.000000000000000000, 0.9238795325112867385, 1.000000000000000000, 0.9238795325112867385, 1.000000000000000000, 0.9238795325112867385, 1.000000000000000000, 0.9238795325112867385, 1.000000000000000000, 0.9238795325112867385, 1.000000000000000000, 0.9238795325112867385, 1.000000000000000000, 0.9238795325112867385, 1.000000000000000000, 0.9238795325112867385, 1.000000000000000000, 0.9238795325112867385, 1.000000000000000000, 0.9238795325112867385, 1.000000000000000000, 0.9238795325112867385, 1.000000000000000000, 0.9238795325112867385, 1.000000000000000000, 0.9238795325112867385, 1.000000000000000000, 0.9238795325112867385, 1.000000000000000000, 0.9238795325112867385, 1.000000000000000000, 0.9238795325112867385, 1.000000000000000000, 0.9238795325112867385, 1.000000000000000000, 0.9238795325112867385, 1.000000000000000000, 0.9238795325112867385, 1.000000000000000000, 0.9238795325112867385, 1.000000000000000000, 0.9238795325112867385, 1.000000000000000000, 0.9238795325112867385, 1.000000000000000000, 0.9238795325112867385, 1.000000000000000000, 0.9238795325112867385, 1.000000000000000000, 0.9238795325112867385, 1.000000000000000000, 0.9238795325112867385, 1.000000000000000000, 0.9238795325112867385, 1.000000000000000000, 0.9238795325112867385, 1.000000000000000000, 0.9238795325112867385, 1.000000000000000000, 0.9238795325112867385, 1.000000000000000000, 0.9238795325112867385, 1.000000000000000000, 0.9238795325112867385, 1.000000000000000000, 0.9238795325112867385, 1.000000000000000000, 0.9238795325112867385, 1.000000000000000000, 0.9238795325112867385, 1.000000000000000000, 0.9238795325112867385, 1.000000000000000000, 0.9238795325112867385, 1.000000000000000000, 0.9238795325112867385, 1.000000000000000000, 0.9238795325112867385, 1.000000000000000000, 0.9238795325112867385, 1.000000000000000000, 0.9238795325112867385, 1.000000000000000000, 0.9238795325112867385, 1.000000000000000000, 0.9238795325112867385, 1.000000000000000000, 0.9238795325112867385, 1.000000000000000000) ) ) 
 REPRESENTATION_ITEM ( '' )  SURFACE ( )  );
#5624 = CARTESIAN_POINT ( 'NONE',  ( 9.920644283265380691E-16, 4.000000000000000000, 18.87500000273119838 ) ) ;
#5625 = VECTOR ( 'NONE', #16118, 1000.000000000000000 ) ;
#5626 = CARTESIAN_POINT ( 'NONE',  ( -3.999999999999999112, 1.656854249492380804, 19.93750000000001066 ) ) ;
#5627 = DIRECTION ( 'NONE',  ( 0.000000000000000000, 0.000000000000000000, -1.000000000000000000 ) ) ;
#5628 = CARTESIAN_POINT ( 'NONE',  ( 9.920644283265380691E-16, 4.000000000000000000, 10.75000000000001066 ) ) ;
#5629 = PLANE ( 'NONE',  #16727 ) ;
#5630 = FILL_AREA_STYLE ('',( #1912 ) ) ;
#5631 = ORIENTED_EDGE ( 'NONE', *, *, #21627, .F. ) ;
#5632 = VECTOR ( 'NONE', #9594, 1000.000000000000000 ) ;
#5633 = CARTESIAN_POINT ( 'NONE',  ( -66.34999999999999432, 7.499999999999995559, 13.96446609406725692 ) ) ;
#5634 = CARTESIAN_POINT ( 'NONE',  ( 6.499999999999999112, 0.000000000000000000, 1.734723475976807094E-15 ) ) ;
#5635 = CARTESIAN_POINT ( 'NONE',  ( 71.85000000109246798, 9.999999999999998224, 12.93301269999999192 ) ) ;
#5636 = CARTESIAN_POINT ( 'NONE',  ( -3.458734124999998993, 1.432654583217640276, 18.37500000136560274 ) ) ;
#5637 = FACE_OUTER_BOUND ( 'NONE', #2927, .T. ) ;
#5638 = CARTESIAN_POINT ( 'NONE',  ( 3.458734125000000770, 1.432654583217640498, -2.449999998634404097 ) ) ;
#5639 = CARTESIAN_POINT ( 'NONE',  ( 4.000000000000000000, 4.898587196589412829E-16, -3.074999997268812901 ) ) ;
#5640 = CARTESIAN_POINT ( 'NONE',  ( 1.432654583217643163, -3.458734124999999437, 11.75000000136560629 ) ) ;
#5641 = CARTESIAN_POINT ( 'NONE',  ( -67.35000000218495586, 8.964466094067256918, 12.49999999999999822 ) ) ;
#5642 = VERTEX_POINT ( 'NONE', #18199 ) ;
#5643 = VECTOR ( 'NONE', #19695, 1000.000000000000000 ) ;
#5644 = CARTESIAN_POINT ( 'NONE',  ( -70.30000000109247082, 12.06698729999999919, 15.85617417291294196 ) ) ;
#5645 = ORIENTED_EDGE ( 'NONE', *, *, #17516, .T. ) ;
#5646 = CARTESIAN_POINT ( 'NONE',  ( 56.87268183416158962, 7.219692298483935566, 12.12345345202367675 ) ) ;
#5647 = CARTESIAN_POINT ( 'NONE',  ( -70.35000000109246798, 11.46158073645647235, 13.53841926354352232 ) ) ;
#5648 = CARTESIAN_POINT ( 'NONE',  ( -3.999999999999998224, -1.656854249492383024, 17.06250000000001066 ) ) ;
#5649 = ORIENTED_EDGE ( 'NONE', *, *, #4218, .F. ) ;
#5650 = CIRCLE ( 'NONE', #1403, 4.000000000000000888 ) ;
#5651 = AXIS2_PLACEMENT_3D ( 'NONE', #7047, #4883, #2956 ) ;
#5652 = EDGE_LOOP ( 'NONE', ( #15517, #21584, #17764, #3536 ) ) ;
#5653 = CARTESIAN_POINT ( 'NONE',  ( -2.445694354108819191, 2.445694354108820523, 19.56250000136560629 ) ) ;
#5654 = CARTESIAN_POINT ( 'NONE',  ( 51.50231816583844591, 12.07320092032949610, 12.83056023321021044 ) ) ;
#5655 = CARTESIAN_POINT ( 'NONE',  ( -65.55000000218494449, 7.499999999999995559, 16.03553390593273420 ) ) ;
#5656 = CIRCLE ( 'NONE', #19044, 5.000000000000000888 ) ;
#5657 = EDGE_CURVE ( 'NONE', #23445, #22997, #16395, .T. ) ;
#5658 = CARTESIAN_POINT ( 'NONE',  ( -71.10000000109246798, 10.85617417291294551, 12.93301269999999370 ) ) ;
#5659 = CARTESIAN_POINT ( 'NONE',  ( -2.445694354108818303, -2.445694354108820967, 11.81250000136560629 ) ) ;
#5660 = DIRECTION ( 'NONE',  ( 0.000000000000000000, -0.000000000000000000, 1.000000000000000000 ) ) ;
#5661 = CARTESIAN_POINT ( 'NONE',  ( 60.24768183416157541, 7.830560233210222876, 17.07320092032950498 ) ) ;
#5662 = DIRECTION ( 'NONE',  ( 1.000000000000000000, 0.000000000000000000, 0.000000000000000000 ) ) ;
#5663 = AXIS2_PLACEMENT_3D ( 'NONE', #1492, #8351, #10636 ) ;
#5664 =( GEOMETRIC_REPRESENTATION_CONTEXT ( 3 ) GLOBAL_UNCERTAINTY_ASSIGNED_CONTEXT ( ( #4986 ) ) GLOBAL_UNIT_ASSIGNED_CONTEXT ( ( #15162, #20630, #2190 ) ) REPRESENTATION_CONTEXT ( 'NONE', 'WORKASPACE' ) );
#5665 = CARTESIAN_POINT ( 'NONE',  ( 51.56250000000000711, 6.999999999999997335, 15.00000000000000533 ) ) ;
#5666 = CARTESIAN_POINT ( 'NONE',  ( 2.828427124746192067, -2.828427124746189847, 17.50000000273119483 ) ) ;
#5667 = EDGE_CURVE ( 'NONE', #18990, #2345, #7326, .T. ) ;
#5668 = CARTESIAN_POINT ( 'NONE',  ( 68.89999999999999147, 9.999999999999998224, 12.49999999999999289 ) ) ;
#5669 = ORIENTED_EDGE ( 'NONE', *, *, #14272, .T. ) ;
#5670 = CARTESIAN_POINT ( 'NONE',  ( 1.236993788156008760E-15, 0.000000000000000000, 21.31370849898476649 ) ) ;
#5671 = CYLINDRICAL_SURFACE ( 'NONE', #1696, 6.735000000000022524 ) ;
#5672 = ORIENTED_EDGE ( 'NONE', *, *, #16360, .F. ) ;
#5673 = CARTESIAN_POINT ( 'NONE',  ( 55.87500000000000711, 7.878679656440349177, 12.87867965644035984 ) ) ;
#5674 = CARTESIAN_POINT ( 'NONE',  ( 1.432654583217639832, 3.458734125000000326, 5.425000001365595459 ) ) ;
#5675 = CARTESIAN_POINT ( 'NONE',  ( 4.999999999999999112, -6.478011392632841314, -6.807171995660652897 ) ) ;
#5676 = EDGE_LOOP ( 'NONE', ( #5776, #18021, #10213, #20303 ) ) ;
#5677 = CARTESIAN_POINT ( 'NONE',  ( 1.656854249492381470, 4.000000000000000000, 15.68750000000001066 ) ) ;
#5678 = AXIS2_PLACEMENT_3D ( 'NONE', #21988, #21639, #9099 ) ;
#5679 = CARTESIAN_POINT ( 'NONE',  ( -2.228340424525890907E-16, 3.639156083333333846, -3.158333332422934348 ) ) ;
#5680 = CARTESIAN_POINT ( 'NONE',  ( 4.000000000000000000, 1.656854249492381248, -3.012499997268812901 ) ) ;
#5681 = ORIENTED_EDGE ( 'NONE', *, *, #15642, .T. ) ;
#5682 = PRODUCT_DEFINITION_SHAPE ( 'NONE', 'NONE',  #23703 ) ;
#5683 = LINE ( 'NONE', #13019, #17112 ) ;
#5684 = AXIS2_PLACEMENT_3D ( 'NONE', #14006, #4765, #15916 ) ;
#5685 = CARTESIAN_POINT ( 'NONE',  ( -2.445694354108819635, -2.445694354108820967, 1.112500001365595681 ) ) ;
#5686 = EDGE_CURVE ( 'NONE', #7993, #20599, #22245, .T. ) ;
#5687 = CARTESIAN_POINT ( 'NONE',  ( 68.79999999999999716, 8.232233047033629347, 13.23223304703362402 ) ) ;
#5688 = EDGE_CURVE ( 'NONE', #2520, #12003, #20136, .T. ) ;
#5689 = VECTOR ( 'NONE', #14262, 1000.000000000000000 ) ;
#5690 = CARTESIAN_POINT ( 'NONE',  ( 1.236993788156008760E-15, 0.000000000000000000, 21.31370849898476649 ) ) ;
#5691 = AXIS2_PLACEMENT_3D ( 'NONE', #12587, #7306, #23334 ) ;
#5692 = LINE ( 'NONE', #13027, #4192 ) ;
#5693 = CARTESIAN_POINT ( 'NONE',  ( 52.53356816583844591, 11.72490539043803004, 18.97181229448534268 ) ) ;
#5694 = CARTESIAN_POINT ( 'NONE',  ( 1.432654583217642275, -3.458734124999999437, 1.050000001365596791 ) ) ;
#5695 = CARTESIAN_POINT ( 'NONE',  ( -2.445694354108818303, -2.445694354108820967, 14.81250000136560452 ) ) ;
#5696 = EDGE_CURVE ( 'NONE', #15755, #3801, #18540, .T. ) ;
#5697 = CARTESIAN_POINT ( 'NONE',  ( -71.70000000000000284, 9.999999999999998224, 17.49999999999999645 ) ) ;
#5698 = CARTESIAN_POINT ( 'NONE',  ( -71.70000000109247651, 7.933012699999995476, 14.14382582708705094 ) ) ;
#5699 = EDGE_CURVE ( 'NONE', #6393, #16436, #23206, .T. ) ;
#5700 = LINE ( 'NONE', #20171, #12099 ) ;
#5701 = ORIENTED_EDGE ( 'NONE', *, *, #21731, .T. ) ;
#5702 = CARTESIAN_POINT ( 'NONE',  ( -2.828427124746189403, 2.828427124746190291, 12.00000000273119660 ) ) ;
#5703 = AXIS2_PLACEMENT_3D ( 'NONE', #19409, #8659, #15959 ) ;
#5704 = DIRECTION ( 'NONE',  ( 0.000000000000000000, 0.000000000000000000, 1.000000000000000000 ) ) ;
#5705 = CARTESIAN_POINT ( 'NONE',  ( -19.99999999999999645, -9.000000000000003553, 10.00000000000008882 ) ) ;
#5706 = VERTEX_POINT ( 'NONE', #13426 ) ;
#5707 = ORIENTED_EDGE ( 'NONE', *, *, #12634, .T. ) ;
#5708 = DIRECTION ( 'NONE',  ( 0.000000000000000000, 0.3090169943749411785, 0.9510565162951557516 ) ) ;
#5709 = CIRCLE ( 'NONE', #8015, 11.00000000000000000 ) ;
#5710 = CARTESIAN_POINT ( 'NONE',  ( 55.59375000000002132, 11.65685424949236015, 10.99999999999998579 ) ) ;
#5711 = VERTEX_POINT ( 'NONE', #11267 ) ;
#5712 = CARTESIAN_POINT ( 'NONE',  ( 4.000000000000000888, 4.898587196589412829E-16, 18.50000000000001066 ) ) ;
#5713 = ORIENTED_EDGE ( 'NONE', *, *, #3228, .F. ) ;
#5714 = CIRCLE ( 'NONE', #4576, 2.500000000000002220 ) ;
#5715 = CARTESIAN_POINT ( 'NONE',  ( 56.18981816583843170, 9.931948859054346102, 10.99999999999999467 ) ) ;
#5716 = EDGE_CURVE ( 'NONE', #611, #12043, #7434, .T. ) ;
#5717 = CARTESIAN_POINT ( 'NONE',  ( 71.10000000109246798, 12.06698730000000275, 15.85617417291294196 ) ) ;
#5718 = AXIS2_PLACEMENT_3D ( 'NONE', #14628, #14863, #21888 ) ;
#5719 = CARTESIAN_POINT ( 'NONE',  ( 4.999999999999997335, 0.000000000000000000, 0.000000000000000000 ) ) ;
#5720 = AXIS2_PLACEMENT_3D ( 'NONE', #19676, #12536, #3400 ) ;
#5721 = CARTESIAN_POINT ( 'NONE',  ( 72.20000000109246230, 10.85617417291294551, 17.06698729999999742 ) ) ;
#5722 = EDGE_CURVE ( 'NONE', #14480, #16157, #16571, .T. ) ;
#5723 = ORIENTED_EDGE ( 'NONE', *, *, #16855, .T. ) ;
#5724 = CARTESIAN_POINT ( 'NONE',  ( 2.828427124746191179, 2.828427124746190291, 16.75000000273119838 ) ) ;
#5725 = DIRECTION ( 'NONE',  ( 0.000000000000000000, -1.000000000000000000, -0.000000000000000000 ) ) ;
#5726 =( BOUNDED_CURVE ( )  B_SPLINE_CURVE ( 2, ( #11984, #4532, #9824, #19252, #815, #17937, #14364, #4763, #16154 ),
 .UNSPECIFIED., .F., .F. ) 
 B_SPLINE_CURVE_WITH_KNOTS ( ( 3, 2, 2, 2, 3 ),
 ( 0.06249999999999961836, 0.07812499999999952816, 0.09374999999999943101, 0.1093749999999993339, 0.1249999999999992367 ),
 .UNSPECIFIED. ) 
 CURVE ( )  GEOMETRIC_REPRESENTATION_ITEM ( )  RATIONAL_B_SPLINE_CURVE ( ( 1.000000000000001776, 0.9238795325112848511, 1.000000000000000000, 0.9238795325112867385, 1.000000000000000000, 0.9238795325112867385, 1.000000000000000000, 0.9238795325112904022, 0.9999999999999963363 ) ) 
 REPRESENTATION_ITEM ( '' )  );
#5727 = CARTESIAN_POINT ( 'NONE',  ( 53.12268183416157541, 12.78030770151606177, 17.87654654797631792 ) ) ;
#5728 = CARTESIAN_POINT ( 'NONE',  ( 3.799967015292484707, 0.6806254479988701478, 2.040000000000004476 ) ) ;
#5729 = CIRCLE ( 'NONE', #14163, 4.000000000000002665 ) ;
#5730 = EDGE_CURVE ( 'NONE', #4949, #839, #5743, .T. ) ;
#5731 = DIRECTION ( 'NONE',  ( 0.000000000000000000, 0.000000000000000000, 1.000000000000000000 ) ) ;
#5732 = CARTESIAN_POINT ( 'NONE',  ( 72.34999999999999432, 12.50000000000000000, 16.03553390593273775 ) ) ;
#5733 = EDGE_CURVE ( 'NONE', #7791, #1264, #20398, .T. ) ;
#5734 = CARTESIAN_POINT ( 'NONE',  ( -67.05000000109247082, 9.999999999999998224, 12.93301269999999192 ) ) ;
#5735 = CARTESIAN_POINT ( 'NONE',  ( -2.974182810908594821, 5.788408252967899514, 4.456522679820626832E-15 ) ) ;
#5736 = ORIENTED_EDGE ( 'NONE', *, *, #10708, .T. ) ;
#5737 = DIRECTION ( 'NONE',  ( 1.224646799147353207E-16, -0.000000000000000000, 1.000000000000000000 ) ) ;
#5738 = CARTESIAN_POINT ( 'NONE',  ( -19.99999999999999645, -9.000000000000003553, 10.00000000000008882 ) ) ;
#5739 = FACE_OUTER_BOUND ( 'NONE', #17470, .T. ) ;
#5740 = CIRCLE ( 'NONE', #4220, 4.000000000000001776 ) ;
#5741 = VERTEX_POINT ( 'NONE', #18791 ) ;
#5742 = FACE_OUTER_BOUND ( 'NONE', #3475, .T. ) ;
#5743 = LINE ( 'NONE', #18666, #1790 ) ;
#5744 = CARTESIAN_POINT ( 'NONE',  ( 0.3198814748697593746, 4.434118497892183264, -0.3507732604232499107 ) ) ;
#5745 = CARTESIAN_POINT ( 'NONE',  ( 38.41764710928345750, -8.974600000000002353, 5.000000000000079936 ) ) ;
#5746 = VERTEX_POINT ( 'NONE', #7546 ) ;
#5747 = CARTESIAN_POINT ( 'NONE',  ( 69.95000000000001705, 12.50000000000000000, 16.03553390593273775 ) ) ;
#5748 = ORIENTED_EDGE ( 'NONE', *, *, #20299, .F. ) ;
#5749 = CYLINDRICAL_SURFACE ( 'NONE', #17920, 2.500000000000009326 ) ;
#5750 = CARTESIAN_POINT ( 'NONE',  ( 1.971781867644420635E-15, -4.000000000000000000, 15.25000000000001066 ) ) ;
#5751 = DIRECTION ( 'NONE',  ( 0.000000000000000000, 0.8090169943749487835, -0.5877852522924714718 ) ) ;
#5752 = DIRECTION ( 'NONE',  ( 0.000000000000000000, 0.000000000000000000, -1.000000000000000000 ) ) ;
#5753 = SURFACE_SIDE_STYLE ('',( #13084 ) ) ;
#5754 = CARTESIAN_POINT ( 'NONE',  ( 70.80000000109245661, 7.933012699999995476, 15.85617417291294196 ) ) ;
#5755 = ORIENTED_EDGE ( 'NONE', *, *, #8429, .T. ) ;
#5756 = VECTOR ( 'NONE', #23229, 1000.000000000000000 ) ;
#5757 = VECTOR ( 'NONE', #6851, 1000.000000000000000 ) ;
#5758 = CARTESIAN_POINT ( 'NONE',  ( -66.54999999999999716, 11.03553390593273598, 12.49999999999999289 ) ) ;
#5759 = VECTOR ( 'NONE', #17269, 1000.000000000000000 ) ;
#5760 = CYLINDRICAL_SURFACE ( 'NONE', #3765, 8.749000000000002331 ) ;
#5761 = EDGE_CURVE ( 'NONE', #21207, #12818, #19008, .T. ) ;
#5762 = CARTESIAN_POINT ( 'NONE',  ( 67.75000000109247367, 11.46158073645647235, 13.53841926354352232 ) ) ;
#5763 = CARTESIAN_POINT ( 'NONE',  ( 1.872352939448454495E-15, -3.458734125000000326, 15.68750000136560629 ) ) ;
#5764 = LINE ( 'NONE', #1796, #14565 ) ;
#5765 = EDGE_CURVE ( 'NONE', #11172, #11370, #16527, .T. ) ;
#5766 = CARTESIAN_POINT ( 'NONE',  ( -1.432654583217641164, -3.458734125000000326, -0.8249999986344030978 ) ) ;
#5767 = CARTESIAN_POINT ( 'NONE',  ( -2.117863837641485618E-16, 3.458734125000000770, -3.262499998634402765 ) ) ;
#5768 = CARTESIAN_POINT ( 'NONE',  ( 13.29415075323381323, -9.000000000000001776, 10.00000000000008882 ) ) ;
#5769 = CARTESIAN_POINT ( 'NONE',  ( -1.432654583217638944, 3.458734125000000326, 15.25000000136560807 ) ) ;
#5770 = DIRECTION ( 'NONE',  ( -1.000000000000000000, 0.000000000000000000, 0.000000000000000000 ) ) ;
#5771 = ORIENTED_EDGE ( 'NONE', *, *, #20199, .F. ) ;
#5772 = CARTESIAN_POINT ( 'NONE',  ( -68.75000000109247367, 11.46158073645647235, 16.46158073645647235 ) ) ;
#5773 = ORIENTED_EDGE ( 'NONE', *, *, #13640, .T. ) ;
#5774 = CARTESIAN_POINT ( 'NONE',  ( 57.56250000000000000, 5.999999999999996447, 15.00000000000001599 ) ) ;
#5775 = CARTESIAN_POINT ( 'NONE',  ( -69.50000000109247367, 10.85617417291294551, 12.93301269999999370 ) ) ;
#5776 = ORIENTED_EDGE ( 'NONE', *, *, #19878, .T. ) ;
#5777 = FACE_OUTER_BOUND ( 'NONE', #8983, .T. ) ;
#5778 = ORIENTED_EDGE ( 'NONE', *, *, #18444, .T. ) ;
#5779 = ORIENTED_EDGE ( 'NONE', *, *, #17180, .T. ) ;
#5780 = CARTESIAN_POINT ( 'NONE',  ( 2.445694354108822299, -2.445694354108820079, 18.06250000136560274 ) ) ;
#5781 = CARTESIAN_POINT ( 'NONE',  ( 55.21875000000000000, 13.00000000000000711, 16.24264068711927322 ) ) ;
#5782 = CARTESIAN_POINT ( 'NONE',  ( -71.40000000109249356, 7.933012699999995476, 15.85617417291294196 ) ) ;
#5783 = CARTESIAN_POINT ( 'NONE',  ( 69.65000000109247935, 9.999999999999998224, 17.06698730000000097 ) ) ;
#5784 = CARTESIAN_POINT ( 'NONE',  ( -69.30000000109247082, 7.933012699999995476, 14.14382582708705094 ) ) ;
#5785 = CARTESIAN_POINT ( 'NONE',  ( 2.445694354108822299, -2.445694354108820079, 11.06250000136560452 ) ) ;
#5786 = CARTESIAN_POINT ( 'NONE',  ( 14.99999999999995559, 15.00000000000000000, -50.00000000000000000 ) ) ;
#5787 = CARTESIAN_POINT ( 'NONE',  ( 53.62500000000000711, 12.12132034355964727, 17.12132034355963484 ) ) ;
#5788 = AXIS2_PLACEMENT_3D ( 'NONE', #10800, #23210, #3106 ) ;
#5789 = DIRECTION ( 'NONE',  ( -0.000000000000000000, -1.000000000000000000, -0.000000000000000000 ) ) ;
#5790 = CARTESIAN_POINT ( 'NONE',  ( -2.445694354108820523, 2.445694354108820523, 5.862500001365596347 ) ) ;
#5791 = CARTESIAN_POINT ( 'NONE',  ( 1.567478505476134606E-15, 4.618802153517012066, -3.433295621305382905 ) ) ;
#5792 = CARTESIAN_POINT ( 'NONE',  ( 1.656854249492381470, 4.000000000000000000, 17.81250000273119483 ) ) ;
#5793 = CARTESIAN_POINT ( 'NONE',  ( -69.25000000218494733, 12.50000000000000000, 16.03553390593273775 ) ) ;
#5794 = ORIENTED_EDGE ( 'NONE', *, *, #22940, .T. ) ;
#5795 = CARTESIAN_POINT ( 'NONE',  ( 70.10000000218494165, 11.76776695296636888, 16.76776695296636532 ) ) ;
#5796 = CARTESIAN_POINT ( 'NONE',  ( -70.45000000000000284, 8.964466094067244484, 12.50000000000000711 ) ) ;
#5797 = ORIENTED_EDGE ( 'NONE', *, *, #13190, .F. ) ;
#5798 = CARTESIAN_POINT ( 'NONE',  ( 54.84375000000000000, 8.757359312880723223, 18.00000000000000355 ) ) ;
#5799 = CARTESIAN_POINT ( 'NONE',  ( -1.432654583217640942, -3.458734124999999882, 3.925000001365594127 ) ) ;
#5800 = PRODUCT_RELATED_PRODUCT_CATEGORY ( 'part', '', ( #127 ) ) ;
#5801 = CARTESIAN_POINT ( 'NONE',  ( 7.010965453233809264, -9.000000000000001776, 10.00000000000008882 ) ) ;
#5802 = ORIENTED_EDGE ( 'NONE', *, *, #15414, .F. ) ;
#5803 = CARTESIAN_POINT ( 'NONE',  ( -3.999999999999999112, 1.656854249492380804, 12.93750000000001243 ) ) ;
#5804 = ADVANCED_FACE ( 'NONE', ( #2128 ), #9463, .T. ) ;
#5805 = CARTESIAN_POINT ( 'NONE',  ( 4.999999999999999112, -1.699438267350438903, 9.241976615262153416 ) ) ;
#5806 = LINE ( 'NONE', #20751, #16378 ) ;
#5807 = ORIENTED_EDGE ( 'NONE', *, *, #17642, .F. ) ;
#5808 = DIRECTION ( 'NONE',  ( 0.000000000000000000, 0.000000000000000000, 1.000000000000000000 ) ) ;
#5809 = CARTESIAN_POINT ( 'NONE',  ( -3.458734125000000770, 0.000000000000000000, -0.01249999863440348635 ) ) ;
#5810 = CARTESIAN_POINT ( 'NONE',  ( 67.04999999999999716, 7.499999999999995559, 16.03553390593273420 ) ) ;
#5811 = DIRECTION ( 'NONE',  ( 0.000000000000000000, 0.000000000000000000, 1.000000000000000000 ) ) ;
#5812 = DIRECTION ( 'NONE',  ( -1.000000000000000000, -0.000000000000000000, 0.000000000000000000 ) ) ;
#5813 = CARTESIAN_POINT ( 'NONE',  ( 54.59606816583844591, 11.58880310854672935, 10.97181229448534445 ) ) ;
#5814 = CARTESIAN_POINT ( 'NONE',  ( -3.458734125000000326, 1.432654583217640276, 0.6750000013655963471 ) ) ;
#5815 = CARTESIAN_POINT ( 'NONE',  ( 1.432654583217643163, -3.458734124999999882, 17.00000000136560629 ) ) ;
#5816 = DIRECTION ( 'NONE',  ( 0.000000000000000000, -0.5877852522924802425, 0.8090169943749422332 ) ) ;
#5817 = CARTESIAN_POINT ( 'NONE',  ( 45.00000000000000000, 10.00000000000001599, 34.11836509645781490 ) ) ;
#5818 = CARTESIAN_POINT ( 'NONE',  ( 4.000000000000000888, 4.898587196589412829E-16, 16.50000000000001066 ) ) ;
#5819 = ORIENTED_EDGE ( 'NONE', *, *, #17341, .F. ) ;
#5820 = CARTESIAN_POINT ( 'NONE',  ( 12.00000000000000000, 0.000000000000000000, -1.469576158976823947E-15 ) ) ;
#5821 = FACE_OUTER_BOUND ( 'NONE', #12451, .T. ) ;
#5822 = CARTESIAN_POINT ( 'NONE',  ( 4.000000000000000888, 4.898587196589412829E-16, 12.50000000000001066 ) ) ;
#5823 = ORIENTED_EDGE ( 'NONE', *, *, #1770, .F. ) ;
#5824 = ORIENTED_EDGE ( 'NONE', *, *, #21761, .T. ) ;
#5825 = EDGE_CURVE ( 'NONE', #3670, #12921, #102, .T. ) ;
#5826 = DIRECTION ( 'NONE',  ( -1.000000000000000000, -4.625929269271486900E-16, 1.224646799147353207E-16 ) ) ;
#5827 = ADVANCED_FACE ( 'NONE', ( #20447 ), #11386, .T. ) ;
#5828 = CARTESIAN_POINT ( 'NONE',  ( 55.03125000000000711, 11.65685424949239923, 18.99999999999998934 ) ) ;
#5829 = ORIENTED_EDGE ( 'NONE', *, *, #16449, .T. ) ;
#5830 = CARTESIAN_POINT ( 'NONE',  ( 2.725741868436127202, -3.045094352033990148, -3.220599429844051453 ) ) ;
#5831 = ORIENTED_EDGE ( 'NONE', *, *, #9670, .T. ) ;
#5832 = CARTESIAN_POINT ( 'NONE',  ( 57.50231816583843170, 12.78030770151603868, 12.12345345202365188 ) ) ;
#5833 = CIRCLE ( 'NONE', #2376, 8.800000000000023803 ) ;
#5834 = EDGE_CURVE ( 'NONE', #2595, #4680, #10298, .T. ) ;
#5835 = CARTESIAN_POINT ( 'NONE',  ( 65.95000000218495018, 12.50000000000000000, 13.96446609406725869 ) ) ;
#5836 = CARTESIAN_POINT ( 'NONE',  ( 66.29999999999999716, 7.499999999999996447, 14.99999999999999645 ) ) ;
#5837 = CARTESIAN_POINT ( 'NONE',  ( 70.20000000109246230, 9.143825827087050939, 12.93301269999999370 ) ) ;
#5838 = VERTEX_POINT ( 'NONE', #10065 ) ;
#5839 = CARTESIAN_POINT ( 'NONE',  ( 1.656854249492381470, 4.000000000000000000, 14.81250000273119483 ) ) ;
#5840 = CARTESIAN_POINT ( 'NONE',  ( 2.828427124746189847, 2.828427124746190291, 0.05000000273118650196 ) ) ;
#5841 = CARTESIAN_POINT ( 'NONE',  ( 52.93518183416157541, 9.931948859054379852, 18.99999999999999289 ) ) ;
#5842 = CARTESIAN_POINT ( 'NONE',  ( 3.250000000000002665, -5.629165124598850767, -3.700000000000000178 ) ) ;
#5843 = LINE ( 'NONE', #18187, #11078 ) ;
#5844 = CARTESIAN_POINT ( 'NONE',  ( 43.27628836966725601, -11.25000000000000355, 10.00000000000008882 ) ) ;
#5845 = DIRECTION ( 'NONE',  ( 1.000000000000000000, 7.703719777548943412E-32, 0.000000000000000000 ) ) ;
#5846 = CARTESIAN_POINT ( 'NONE',  ( -2.149058192116894084, 6.264794173742276762, -0.06682554136337909290 ) ) ;
#5847 = ORIENTED_EDGE ( 'NONE', *, *, #20642, .T. ) ;
#5848 = DIRECTION ( 'NONE',  ( -1.000000000000000000, -0.000000000000000000, -0.000000000000000000 ) ) ;
#5849 = CARTESIAN_POINT ( 'NONE',  ( 52.78125000000000000, 8.757359312880703683, 11.99999999999999822 ) ) ;
#5850 = EDGE_CURVE ( 'NONE', #6494, #22779, #11746, .T. ) ;
#5851 = CYLINDRICAL_SURFACE ( 'NONE', #16176, 11.00000000000000000 ) ;
#5852 = FILL_AREA_STYLE ('',( #3817 ) ) ;
#5853 = ORIENTED_EDGE ( 'NONE', *, *, #6567, .T. ) ;
#5854 = CARTESIAN_POINT ( 'NONE',  ( 27.50000000000000000, 4.500000000000006217, -36.31025403784446581 ) ) ;
#5855 = DIRECTION ( 'NONE',  ( 0.000000000000000000, 0.000000000000000000, 1.000000000000000000 ) ) ;
#5856 = CARTESIAN_POINT ( 'NONE',  ( 1.654252653721905331, 3.663718938583014229, -0.01223254789873410957 ) ) ;
#5857 = CONICAL_SURFACE ( 'NONE', #19234, 6.500000000000000888, 1.047197551196596521 ) ;
#5858 = EDGE_CURVE ( 'NONE', #17335, #6815, #9821, .T. ) ;
#5859 = CARTESIAN_POINT ( 'NONE',  ( -2.828427124746190291, 2.828427124746190291, -2.824999999999997513 ) ) ;
#5860 = VERTEX_POINT ( 'NONE', #20804 ) ;
#5861 = DIRECTION ( 'NONE',  ( 0.000000000000000000, -1.000000000000000000, 0.000000000000000000 ) ) ;
#5862 = ORIENTED_EDGE ( 'NONE', *, *, #22193, .F. ) ;
#5863 = CARTESIAN_POINT ( 'NONE',  ( 1.600000000000004086, 0.000000000000000000, 0.000000000000000000 ) ) ;
#5864 = CARTESIAN_POINT ( 'NONE',  ( 1.656854249492384135, -3.999999999999999112, 14.31250000000001066 ) ) ;
#5865 = EDGE_CURVE ( 'NONE', #21100, #2825, #2602, .T. ) ;
#5866 = DIRECTION ( 'NONE',  ( 0.3420201433256622736, -0.9396926207859106484, -1.232595164407828100E-31 ) ) ;
#5867 = EDGE_CURVE ( 'NONE', #2957, #11847, #4529, .T. ) ;
#5868 = DIRECTION ( 'NONE',  ( 0.000000000000000000, 0.000000000000000000, 1.000000000000000000 ) ) ;
#5869 =( BOUNDED_CURVE ( )  B_SPLINE_CURVE ( 2, ( #3482, #7336, #7443, #19757, #5628 ),
 .UNSPECIFIED., .F., .F. ) 
 B_SPLINE_CURVE_WITH_KNOTS ( ( 3, 2, 3 ),
 ( 0.9000000000000000222, 0.9124999999999999778, 0.9250000000000000444 ),
 .UNSPECIFIED. ) 
 CURVE ( )  GEOMETRIC_REPRESENTATION_ITEM ( )  RATIONAL_B_SPLINE_CURVE ( ( 1.000000000000000000, 0.9238795325112867385, 1.000000000000000000, 0.9238795325112867385, 1.000000000000000000 ) ) 
 REPRESENTATION_ITEM ( '' )  );
#5870 = DIRECTION ( 'NONE',  ( -1.000000000000000000, -0.000000000000000000, -0.000000000000000000 ) ) ;
#5871 = CARTESIAN_POINT ( 'NONE',  ( 69.10000000109246798, 9.143825827087049163, 17.06698730000000097 ) ) ;
#5872 = ORIENTED_EDGE ( 'NONE', *, *, #15308, .F. ) ;
#5873 = VECTOR ( 'NONE', #5382, 1000.000000000000000 ) ;
#5874 = DIRECTION ( 'NONE',  ( -1.000000000000000000, 0.000000000000000000, 0.000000000000000000 ) ) ;
#5875 = TOROIDAL_SURFACE ( 'NONE', #521, 6.200000000000020606, 0.1999999999999997613 ) ;
#5876 = CARTESIAN_POINT ( 'NONE',  ( -72.50000000000000000, 9.999999999999998224, 14.99999999999999645 ) ) ;
#5877 = CARTESIAN_POINT ( 'NONE',  ( 71.80000000109245661, 9.143825827087050939, 12.93301269999999370 ) ) ;
#5878 = CARTESIAN_POINT ( 'NONE',  ( 3.458734125000001214, 1.432654583217640498, 19.00000000136560629 ) ) ;
#5879 = CARTESIAN_POINT ( 'NONE',  ( -10.00000000000000000, 0.000000000000000000, 0.000000000000000000 ) ) ;
#5880 = DIRECTION ( 'NONE',  ( 0.000000000000000000, -0.5000000000000009992, -0.8660254037844380415 ) ) ;
#5881 = CARTESIAN_POINT ( 'NONE',  ( 1.656854249492380360, 4.000000000000000000, 0.9875000000000008216 ) ) ;
#5882 = CARTESIAN_POINT ( 'NONE',  ( -71.15000000218496723, 7.499999999999996447, 16.03553390593273775 ) ) ;
#5883 = CARTESIAN_POINT ( 'NONE',  ( -2.445694354108818303, -2.445694354108820523, 14.56250000136560452 ) ) ;
#5884 = DIRECTION ( 'NONE',  ( -1.000000000000000000, 0.000000000000000000, 0.000000000000000000 ) ) ;
#5885 = PRODUCT_DEFINITION_SHAPE ( 'NONE', 'NONE',  #23700 ) ;
#5886 = ORIENTED_EDGE ( 'NONE', *, *, #11859, .F. ) ;
#5887 = CARTESIAN_POINT ( 'NONE',  ( -69.05000000109247082, 7.933012699999995476, 14.99999999999999645 ) ) ;
#5888 = ORIENTED_EDGE ( 'NONE', *, *, #20061, .T. ) ;
#5889 = CARTESIAN_POINT ( 'NONE',  ( 59.53125000000000000, 11.65685424949239923, 18.99999999999998934 ) ) ;
#5890 = CARTESIAN_POINT ( 'NONE',  ( -71.10000000109246798, 10.85617417291294551, 12.93301269999999370 ) ) ;
#5891 = APPLICATION_PROTOCOL_DEFINITION ( 'draft international standard', 'automotive_design', 1998, #9014 ) ;
#5892 = ADVANCED_BREP_SHAPE_REPRESENTATION ( '', ( #6561, #7318 ), #21755 ) ;
#5893 = ORIENTED_EDGE ( 'NONE', *, *, #3532, .F. ) ;
#5894 = PLANE ( 'NONE',  #16654 ) ;
#5895 = ORIENTED_EDGE ( 'NONE', *, *, #10123, .T. ) ;
#5896 = EDGE_CURVE ( 'NONE', #13541, #1913, #690, .T. ) ;
#5897 = ORIENTED_EDGE ( 'NONE', *, *, #2134, .T. ) ;
#5898 = CARTESIAN_POINT ( 'NONE',  ( 3.458734125000001658, 4.235727675282972223E-16, 16.18750000136560629 ) ) ;
#5899 = EDGE_CURVE ( 'NONE', #19009, #12570, #13890, .T. ) ;
#5900 = CARTESIAN_POINT ( 'NONE',  ( 52.87500000000000711, 7.878679656440349177, 12.87867965644035984 ) ) ;
#5901 = EDGE_CURVE ( 'NONE', #438, #21232, #9150, .T. ) ;
#5902 = CARTESIAN_POINT ( 'NONE',  ( -68.55000000109247082, 11.46158073645647235, 13.53841926354352232 ) ) ;
#5903 = CARTESIAN_POINT ( 'NONE',  ( 68.50000000109247367, 10.85617417291294551, 12.93301269999999192 ) ) ;
#5904 = CARTESIAN_POINT ( 'NONE',  ( -68.30000000109247082, 9.143825827087049163, 17.06698729999999742 ) ) ;
#5905 = DIRECTION ( 'NONE',  ( 0.000000000000000000, 0.000000000000000000, 1.000000000000000000 ) ) ;
#5906 = CARTESIAN_POINT ( 'NONE',  ( 57.24768183416158962, 7.830560233210222876, 17.07320092032950498 ) ) ;
#5907 = FACE_OUTER_BOUND ( 'NONE', #7523, .T. ) ;
#5908 = CARTESIAN_POINT ( 'NONE',  ( 2.445694354108820967, -2.445694354108820079, 4.362500001365595459 ) ) ;
#5909 = CARTESIAN_POINT ( 'NONE',  ( 2.290893957444128645E-15, 4.647089433458768681, -3.572167766733382877 ) ) ;
#5910 = CARTESIAN_POINT ( 'NONE',  ( -2.828427124746188515, -2.828427124746190735, 15.25000000273119660 ) ) ;
#5911 = CARTESIAN_POINT ( 'NONE',  ( -69.15000000218495302, 12.50000000000000000, 13.96446609406725692 ) ) ;
#5912 = ORIENTED_EDGE ( 'NONE', *, *, #13607, .F. ) ;
#5913 = FACE_OUTER_BOUND ( 'NONE', #14977, .T. ) ;
#5914 = VERTEX_POINT ( 'NONE', #13651 ) ;
#5915 = CARTESIAN_POINT ( 'NONE',  ( 57.99768183416157541, 12.16943976678977535, 12.92679907967048614 ) ) ;
#5916 = CARTESIAN_POINT ( 'NONE',  ( -3.458734125000000326, 1.432654583217640276, 1.675000001365597235 ) ) ;
#5917 = CIRCLE ( 'NONE', #23496, 2.500000000000000444 ) ;
#5918 = CARTESIAN_POINT ( 'NONE',  ( 1.025207404391860050E-15, 3.458734125000000326, 10.18750000136560629 ) ) ;
#5919 = VERTEX_POINT ( 'NONE', #1159 ) ;
#5920 = CARTESIAN_POINT ( 'NONE',  ( 9.920644283265380691E-16, 4.000000000000000000, 13.75000000000001066 ) ) ;
#5921 = CARTESIAN_POINT ( 'NONE',  ( -2.828427124746189403, -2.828427124746190735, -2.574999999999999289 ) ) ;
#5922 = AXIS2_PLACEMENT_3D ( 'NONE', #15042, #20026, #20384 ) ;
#5923 = ADVANCED_FACE ( 'NONE', ( #19138 ), #6784, .T. ) ;
#5924 = VECTOR ( 'NONE', #8746, 1000.000000000000000 ) ;
#5925 = DIRECTION ( 'NONE',  ( 0.000000000000000000, 0.9510565162951544194, -0.3090169943749446202 ) ) ;
#5926 = VERTEX_POINT ( 'NONE', #4409 ) ;
#5927 = CARTESIAN_POINT ( 'NONE',  ( -69.05000000218494449, 11.03553390593273598, 12.49999999999999289 ) ) ;
#5928 = CARTESIAN_POINT ( 'NONE',  ( -2.117863837641485618E-16, 3.458734125000000770, 1.737500001365596347 ) ) ;
#5929 = CARTESIAN_POINT ( 'NONE',  ( 68.59999999999999432, 8.232233047033627571, 16.76776695296636532 ) ) ;
#5930 = CARTESIAN_POINT ( 'NONE',  ( 0.000000000000000000, -0.4999240074893842034, -8.734705317681632053 ) ) ;
#5931 = ADVANCED_FACE ( 'NONE', ( #15694 ), #813, .F. ) ;
#5933 = DIRECTION ( 'NONE',  ( 0.000000000000000000, 0.000000000000000000, -1.000000000000000000 ) ) ;
#5932 = VECTOR ( 'NONE', #7325, 1000.000000000000114 ) ;
#5934 = CARTESIAN_POINT ( 'NONE',  ( 50.93981816583844591, 10.06805114094564857, 19.00000000000000000 ) ) ;
#5935 = AXIS2_PLACEMENT_3D ( 'NONE', #182, #8849, #21615 ) ;
#5936 = CARTESIAN_POINT ( 'NONE',  ( 3.458734125000000770, 4.235727675282972223E-16, 4.487500001365595459 ) ) ;
#5937 = CARTESIAN_POINT ( 'NONE',  ( -3.458734124999999437, 0.000000000000000000, 16.68750000136560629 ) ) ;
#5938 = CARTESIAN_POINT ( 'NONE',  ( 68.75000000218494733, 7.499999999999996447, 16.03553390593273775 ) ) ;
#5939 = CARTESIAN_POINT ( 'NONE',  ( -70.55000000109245661, 11.46158073645647235, 16.46158073645647235 ) ) ;
#5940 = CARTESIAN_POINT ( 'NONE',  ( -69.95000000000001705, 12.50000000000000000, 16.03553390593273775 ) ) ;
#5941 = ORIENTED_EDGE ( 'NONE', *, *, #19677, .F. ) ;
#5942 = CARTESIAN_POINT ( 'NONE',  ( 4.000000000000001776, -1.656854249492379694, 14.43750000000001066 ) ) ;
#5943 = DIRECTION ( 'NONE',  ( 0.000000000000000000, 0.000000000000000000, -1.000000000000000000 ) ) ;
#5944 = CARTESIAN_POINT ( 'NONE',  ( -71.15000000109247935, 11.46158073645647235, 16.46158073645647235 ) ) ;
#5945 = ORIENTED_EDGE ( 'NONE', *, *, #21430, .T. ) ;
#5946 = APPLICATION_CONTEXT ( 'automotive_design' ) ;
#5947 = VERTEX_POINT ( 'NONE', #8500 ) ;
#5948 = CARTESIAN_POINT ( 'NONE',  ( 4.999999999999999112, 0.000000000000000000, 0.000000000000000000 ) ) ;
#5949 = CARTESIAN_POINT ( 'NONE',  ( 60.00000000000000000, 9.999999999999998224, 17.49999999999999645 ) ) ;
#5950 = EDGE_LOOP ( 'NONE', ( #21380, #20887, #1812, #23096, #18205 ) ) ;
#5951 = CARTESIAN_POINT ( 'NONE',  ( 0.000000000000000000, 0.000000000000000000, 19.04999999999996874 ) ) ;
#5952 = EDGE_LOOP ( 'NONE', ( #2482, #9297, #8377, #13464 ) ) ;
#5953 = CARTESIAN_POINT ( 'NONE',  ( 56.56481816583843170, 5.999999999999996447, 15.06805114094564502 ) ) ;
#5954 = VECTOR ( 'NONE', #15610, 1000.000000000000000 ) ;
#5955 = CARTESIAN_POINT ( 'NONE',  ( 71.15000000109247935, 11.46158073645647235, 16.46158073645647235 ) ) ;
#5956 = CARTESIAN_POINT ( 'NONE',  ( -3.999999999999999112, 1.656854249492380804, 19.93750000000001066 ) ) ;
#5957 = CARTESIAN_POINT ( 'NONE',  ( 71.85000000109246798, 9.999999999999998224, 12.93301269999999192 ) ) ;
#5958 = ORIENTED_EDGE ( 'NONE', *, *, #9461, .T. ) ;
#5959 = CARTESIAN_POINT ( 'NONE',  ( -2.828427124746189403, 2.828427124746190291, 13.00000000273119660 ) ) ;
#5960 = AXIS2_PLACEMENT_3D ( 'NONE', #4296, #17357, #17476 ) ;
#5961 = VECTOR ( 'NONE', #4437, 1000.000000000000000 ) ;
#5962 = EDGE_CURVE ( 'NONE', #4764, #22004, #3760, .T. ) ;
#5963 = CARTESIAN_POINT ( 'NONE',  ( 0.000000000000000000, 7.360373001730918574, 4.729683950898897038 ) ) ;
#5964 = CARTESIAN_POINT ( 'NONE',  ( 54.81018183416157541, 14.00000000000000000, 15.06805114094561304 ) ) ;
#5965 = CARTESIAN_POINT ( 'NONE',  ( 0.000000000000000000, 0.000000000000000000, 20.00000000000001066 ) ) ;
#5966 = CARTESIAN_POINT ( 'NONE',  ( 5.000000000000000888, 4.250000000000000000, 0.000000000000000000 ) ) ;
#5967 = DIRECTION ( 'NONE',  ( 0.000000000000000000, -1.000000000000000000, 0.000000000000000000 ) ) ;
#5968 = FACE_OUTER_BOUND ( 'NONE', #22405, .T. ) ;
#5969 = CARTESIAN_POINT ( 'NONE',  ( 4.999999999999999112, 9.680994141368847394, -5.222868219166749704 ) ) ;
#5970 = EDGE_LOOP ( 'NONE', ( #11130, #11714, #15199, #78 ) ) ;
#5971 = CARTESIAN_POINT ( 'NONE',  ( 52.40625000000000000, 12.99999999999999645, 13.75735931288070191 ) ) ;
#5972 = CARTESIAN_POINT ( 'NONE',  ( -70.75000000000000000, 12.50000000000000000, 16.03553390593273775 ) ) ;
#5973 = ADVANCED_FACE ( 'NONE', ( #6215, #15457 ), #22967, .F. ) ;
#5974 = ORIENTED_EDGE ( 'NONE', *, *, #2562, .F. ) ;
#5975 = CARTESIAN_POINT ( 'NONE',  ( 2.828427124746191179, 2.828427124746190291, 14.75000000273119660 ) ) ;
#5976 = LINE ( 'NONE', #9952, #6259 ) ;
#5977 = CARTESIAN_POINT ( 'NONE',  ( -70.85000000218494165, 12.50000000000000000, 16.03553390593273775 ) ) ;
#5978 = EDGE_LOOP ( 'NONE', ( #23320, #22301, #15007, #4560 ) ) ;
#5979 = FACE_BOUND ( 'NONE', #21559, .T. ) ;
#5980 = VERTEX_POINT ( 'NONE', #20913 ) ;
#5981 = CARTESIAN_POINT ( 'NONE',  ( -4.000000000000000000, 0.000000000000000000, 1.300000000000000711 ) ) ;
#5982 = CARTESIAN_POINT ( 'NONE',  ( -1.656854249492380138, -3.999999999999999112, 13.18750000000001243 ) ) ;
#5983 = CARTESIAN_POINT ( 'NONE',  ( 28.81814781032300488, 8.768352694965047434, 10.00000000000008882 ) ) ;
#5984 = EDGE_CURVE ( 'NONE', #8553, #9649, #15579, .T. ) ;
#5985 = DIRECTION ( 'NONE',  ( 1.000000000000000000, 0.000000000000000000, -0.000000000000000000 ) ) ;
#5986 = FACE_OUTER_BOUND ( 'NONE', #11546, .T. ) ;
#5987 = CARTESIAN_POINT ( 'NONE',  ( 70.45000000109247651, 12.06698730000000097, 14.99999999999999645 ) ) ;
#5988 = ORIENTED_EDGE ( 'NONE', *, *, #14910, .T. ) ;
#5989 = EDGE_CURVE ( 'NONE', #17013, #8404, #1555, .T. ) ;
#5990 = LINE ( 'NONE', #13551, #16425 ) ;
#5991 = EDGE_CURVE ( 'NONE', #13512, #21587, #14918, .T. ) ;
#5992 = CARTESIAN_POINT ( 'NONE',  ( -2.000000000000001776, 9.887492094615969966E-16, 8.073750000000021743 ) ) ;
#5993 = CARTESIAN_POINT ( 'NONE',  ( 66.15000000109247935, 11.46158073645647235, 13.53841926354352232 ) ) ;
#5994 = CARTESIAN_POINT ( 'NONE',  ( -1.432654583217638944, 3.458734125000000326, 15.25000000136560807 ) ) ;
#5995 = CARTESIAN_POINT ( 'NONE',  ( 35.00000000000000000, 4.500000000000001776, -20.00000000000000355 ) ) ;
#5996 = CARTESIAN_POINT ( 'NONE',  ( -3.458734125000000326, -1.432654583217642497, -0.9499999986344030978 ) ) ;
#5997 = CARTESIAN_POINT ( 'NONE',  ( 2.828427124746189847, 2.828427124746190291, 2.925000000000002043 ) ) ;
#5998 = CARTESIAN_POINT ( 'NONE',  ( 1.656854249492381470, 4.000000000000000000, 12.68750000000001066 ) ) ;
#5999 = CARTESIAN_POINT ( 'NONE',  ( 1.025207404391860050E-15, 3.458734125000000326, 14.18750000136560452 ) ) ;
#6000 = DIRECTION ( 'NONE',  ( 0.3420201433256622181, 0.9396926207859107594, -6.162975822039141593E-32 ) ) ;
#6001 = EDGE_CURVE ( 'NONE', #7167, #6956, #7294, .T. ) ;
#6002 = ADVANCED_FACE ( 'NONE', ( #19714 ), #18169, .T. ) ;
#6003 = VERTEX_POINT ( 'NONE', #16268 ) ;
#6004 = CARTESIAN_POINT ( 'NONE',  ( 4.000000000000000888, 4.898587196589412829E-16, 15.62500000273119660 ) ) ;
#6005 = ORIENTED_EDGE ( 'NONE', *, *, #1743, .F. ) ;
#6006 = VECTOR ( 'NONE', #14444, 1000.000000000000000 ) ;
#6007 = CARTESIAN_POINT ( 'NONE',  ( 58.40625000000000711, 13.99999999999999289, 13.34314575050759544 ) ) ;
#6008 = CARTESIAN_POINT ( 'NONE',  ( -72.20000000109246230, 10.85617417291294551, 17.06698729999999742 ) ) ;
#6009 = SHAPE_DEFINITION_REPRESENTATION ( #14894, #1939 ) ;
#6010 = ORIENTED_EDGE ( 'NONE', *, *, #13216, .F. ) ;
#6011 = DIRECTION ( 'NONE',  ( -1.000000000000000000, 0.000000000000000000, 0.000000000000000000 ) ) ;
#6012 = ORIENTED_EDGE ( 'NONE', *, *, #8298, .F. ) ;
#6013 = ORIENTED_EDGE ( 'NONE', *, *, #13779, .F. ) ;
#6014 = CARTESIAN_POINT ( 'NONE',  ( -3.458734124999998993, -1.432654583217642497, 17.75000000136560629 ) ) ;
#6015 = CARTESIAN_POINT ( 'NONE',  ( 58.68750000000000000, 9.999999999999989342, 11.99999999999999467 ) ) ;
#6016 = VECTOR ( 'NONE', #1370, 1000.000000000000000 ) ;
#6017 = CARTESIAN_POINT ( 'NONE',  ( -66.70000000109246230, 7.933012699999995476, 14.14382582708705094 ) ) ;
#6018 = CARTESIAN_POINT ( 'NONE',  ( 69.05000000109247082, 7.933012699999995476, 14.99999999999999645 ) ) ;
#6019 = CARTESIAN_POINT ( 'NONE',  ( -66.00000000109245946, 7.933012699999995476, 15.85617417291294196 ) ) ;
#6020 = ADVANCED_FACE ( 'NONE', ( #6803, #23558, #14123 ), #21387, .F. ) ;
#6021 = CARTESIAN_POINT ( 'NONE',  ( 0.000000000000000000, 4.762163868918413812, -9.915734732513168836 ) ) ;
#6022 = CARTESIAN_POINT ( 'NONE',  ( 55.09143183416158962, 11.31069182806491291, 12.02818770551463778 ) ) ;
#6023 = CYLINDRICAL_SURFACE ( 'NONE', #20764, 4.000000000000001776 ) ;
#6024 = VECTOR ( 'NONE', #11816, 1000.000000000000000 ) ;
#6025 = CARTESIAN_POINT ( 'NONE',  ( 3.458734125000000770, 1.432654583217640498, 4.550000001365596347 ) ) ;
#6026 = CARTESIAN_POINT ( 'NONE',  ( -2.445694354108819191, 2.445694354108820523, 12.31250000136560629 ) ) ;
#6027 = CARTESIAN_POINT ( 'NONE',  ( -1.656854249492379250, 4.000000000000000000, 17.93750000273119483 ) ) ;
#6028 = CARTESIAN_POINT ( 'NONE',  ( 14.99999999999999289, 10.00000000000000000, -50.00000000000000000 ) ) ;
#6029 = VECTOR ( 'NONE', #18872, 1000.000000000000000 ) ;
#6030 = VECTOR ( 'NONE', #18057, 1000.000000000000000 ) ;
#6031 = EDGE_CURVE ( 'NONE', #5128, #16266, #1385, .T. ) ;
#6032 = ORIENTED_EDGE ( 'NONE', *, *, #16551, .F. ) ;
#6033 = CARTESIAN_POINT ( 'NONE',  ( -1.656854249492379472, 4.000000000000000000, 13.81250000000001066 ) ) ;
#6034 = ORIENTED_EDGE ( 'NONE', *, *, #10964, .T. ) ;
#6035 = CARTESIAN_POINT ( 'NONE',  ( 57.15393183416157541, 6.971812294485357775, 16.17458954617365663 ) ) ;
#6036 = CARTESIAN_POINT ( 'NONE',  ( -1.432654583217640276, 3.458734125000000326, 1.550000001365597013 ) ) ;
#6037 = CARTESIAN_POINT ( 'NONE',  ( 0.000000000000000000, 0.000000000000000000, 0.000000000000000000 ) ) ;
#6038 = ORIENTED_EDGE ( 'NONE', *, *, #671, .T. ) ;
#6039 = CARTESIAN_POINT ( 'NONE',  ( 4.000000000000000888, 4.898587196589412829E-16, 11.50000000000001066 ) ) ;
#6040 = DIRECTION ( 'NONE',  ( -1.000000000000000000, 0.000000000000000000, 0.000000000000000000 ) ) ;
#6041 = DIRECTION ( 'NONE',  ( -1.000000000000000000, -0.000000000000000000, 0.000000000000000000 ) ) ;
#6042 = VERTEX_POINT ( 'NONE', #3553 ) ;
#6043 = VECTOR ( 'NONE', #10899, 1000.000000000000000 ) ;
#6044 = CARTESIAN_POINT ( 'NONE',  ( -70.00000000218494733, 12.50000000000000000, 14.99999999999999645 ) ) ;
#6045 = CARTESIAN_POINT ( 'NONE',  ( 3.458734125000001214, -1.432654583217639610, -2.574999998634404541 ) ) ;
#6046 = AXIS2_PLACEMENT_3D ( 'NONE', #10281, #23293, #23055 ) ;
#6047 = CIRCLE ( 'NONE', #23246, 8.749000000000002331 ) ;
#6048 = DIRECTION ( 'NONE',  ( 1.000000000000000000, -0.000000000000000000, -0.000000000000000000 ) ) ;
#6049 = CARTESIAN_POINT ( 'NONE',  ( 68.49999999999998579, 9.999999999999998224, 17.49999999999999645 ) ) ;
#6050 = CARTESIAN_POINT ( 'NONE',  ( 4.000000000000001776, -1.656854249492379694, 11.43750000000001066 ) ) ;
#6051 = DIRECTION ( 'NONE',  ( -1.000000000000000000, -0.000000000000000000, -0.000000000000000000 ) ) ;
#6052 = CARTESIAN_POINT ( 'NONE',  ( 56.93981816583843170, 10.06805114094563791, 17.99999999999999645 ) ) ;
#6053 = CARTESIAN_POINT ( 'NONE',  ( -3.458734125000000326, -1.432654583217642497, 4.050000001365596347 ) ) ;
#6054 = CARTESIAN_POINT ( 'NONE',  ( 1.432654583217643163, -3.458734124999999882, 14.00000000136560629 ) ) ;
#6055 = EDGE_CURVE ( 'NONE', #3223, #22912, #1425, .T. ) ;
#6056 = CARTESIAN_POINT ( 'NONE',  ( 68.80000000218494449, 7.499999999999996447, 14.99999999999999645 ) ) ;
#6057 = CARTESIAN_POINT ( 'NONE',  ( -70.35000000109246798, 11.46158073645647235, 13.53841926354352232 ) ) ;
#6058 = LINE ( 'NONE', #11115, #18959 ) ;
#6059 = ORIENTED_EDGE ( 'NONE', *, *, #5699, .T. ) ;
#6060 = CARTESIAN_POINT ( 'NONE',  ( 2.500000000000000000, 0.000000000000000000, 0.000000000000000000 ) ) ;
#6061 = CARTESIAN_POINT ( 'NONE',  ( -4.000000000000000000, 0.000000000000000000, 2.425000002731188431 ) ) ;
#6062 = CARTESIAN_POINT ( 'NONE',  ( -70.40000000109250777, 10.85617417291294551, 17.06698729999999742 ) ) ;
#6063 = ORIENTED_EDGE ( 'NONE', *, *, #3662, .T. ) ;
#6064 = ORIENTED_EDGE ( 'NONE', *, *, #743, .T. ) ;
#6065 = VECTOR ( 'NONE', #21147, 1000.000000000000000 ) ;
#6066 = AXIS2_PLACEMENT_3D ( 'NONE', #6275, #13592, #20859 ) ;
#6067 = CARTESIAN_POINT ( 'NONE',  ( 38.42689195323381313, -9.000000000000001776, 5.000000000000079936 ) ) ;
#6068 = EDGE_LOOP ( 'NONE', ( #19811, #18285, #20981, #5564 ) ) ;
#6069 = FACE_OUTER_BOUND ( 'NONE', #17881, .T. ) ;
#6070 = AXIS2_PLACEMENT_3D ( 'NONE', #8078, #22890, #8430 ) ;
#6071 = CARTESIAN_POINT ( 'NONE',  ( 69.90000000109247935, 7.933012699999995476, 14.14382582708705094 ) ) ;
#6072 = AXIS2_PLACEMENT_3D ( 'NONE', #12052, #14315, #15872 ) ;
#6073 = CARTESIAN_POINT ( 'NONE',  ( 4.000000000000000000, 4.898587196589412829E-16, -2.074999997268812013 ) ) ;
#6074 = VERTEX_POINT ( 'NONE', #8725 ) ;
#6075 = PLANE ( 'NONE',  #22466 ) ;
#6076 = VERTEX_POINT ( 'NONE', #19597 ) ;
#6077 = CARTESIAN_POINT ( 'NONE',  ( -2.828427124746189403, 2.828427124746190291, 12.00000000273119660 ) ) ;
#6078 = VECTOR ( 'NONE', #20419, 1000.000000000000000 ) ;
#6079 = CARTESIAN_POINT ( 'NONE',  ( 57.84375000000000711, 8.343145750507638070, 19.00000000000000711 ) ) ;
#6080 = CARTESIAN_POINT ( 'NONE',  ( 20.49585944720908870, 5.739287449811636854, 10.00000000000008882 ) ) ;
#6081 = CARTESIAN_POINT ( 'NONE',  ( 3.458734125000002102, -1.432654583217639610, 16.87500000136560629 ) ) ;
#6082 = DIRECTION ( 'NONE',  ( 0.000000000000000000, 0.000000000000000000, -1.000000000000000000 ) ) ;
#6083 = CARTESIAN_POINT ( 'NONE',  ( 4.000000000000000888, -1.656854249492379694, 0.7375000000000022649 ) ) ;
#6084 = ORIENTED_EDGE ( 'NONE', *, *, #1335, .F. ) ;
#6085 = DIRECTION ( 'NONE',  ( 0.3373062947069096484, -0.9413949561959079615, -4.130810741450707148E-17 ) ) ;
#6086 = ORIENTED_EDGE ( 'NONE', *, *, #6871, .T. ) ;
#6087 = CARTESIAN_POINT ( 'NONE',  ( 40.95362874676621345, -9.000000000000005329, 10.00000000000008882 ) ) ;
#6088 = CARTESIAN_POINT ( 'NONE',  ( -3.847601380332740018, -11.25000000000000355, 10.00000000000008882 ) ) ;
#6089 = AXIS2_PLACEMENT_3D ( 'NONE', #9613, #9141, #19992 ) ;
#6090 = ORIENTED_EDGE ( 'NONE', *, *, #9929, .F. ) ;
#6091 = CIRCLE ( 'NONE', #17956, 6.735000000000022524 ) ;
#6092 = LINE ( 'NONE', #15218, #18542 ) ;
#6093 = CARTESIAN_POINT ( 'NONE',  ( 2.000000000000001776, 0.000000000000000000, 0.000000000000000000 ) ) ;
#6094 = CARTESIAN_POINT ( 'NONE',  ( 0.000000000000000000, 0.000000000000000000, 0.000000000000000000 ) ) ;
#6095 = CARTESIAN_POINT ( 'NONE',  ( -70.65000000218495302, 11.03553390593268269, 12.49999999999994138 ) ) ;
#6096 = ORIENTED_EDGE ( 'NONE', *, *, #4248, .T. ) ;
#6097 = LINE ( 'NONE', #8264, #19462 ) ;
#6098 = ORIENTED_EDGE ( 'NONE', *, *, #15236, .F. ) ;
#6099 = AXIS2_PLACEMENT_3D ( 'NONE', #18110, #18225, #23380 ) ;
#6100 = EDGE_CURVE ( 'NONE', #17999, #1835, #10888, .T. ) ;
#6101 = CARTESIAN_POINT ( 'NONE',  ( 71.60000000109246798, 9.143825827087052716, 12.93301269999999192 ) ) ;
#6102 = AXIS2_PLACEMENT_3D ( 'NONE', #21085, #3006, #19647 ) ;
#6103 = CARTESIAN_POINT ( 'NONE',  ( 4.000000000000000888, 1.656854249492381248, 13.56250000000001066 ) ) ;
#6104 = DIRECTION ( 'NONE',  ( -7.087422195345011518E-32, -1.000000000000000000, -0.000000000000000000 ) ) ;
#6105 = ORIENTED_EDGE ( 'NONE', *, *, #22819, .T. ) ;
#6106 = DIRECTION ( 'NONE',  ( -1.000000000000000000, -0.000000000000000000, -0.000000000000000000 ) ) ;
#6107 = CARTESIAN_POINT ( 'NONE',  ( 0.000000000000000000, 0.000000000000000000, 0.000000000000000000 ) ) ;
#6108 = CARTESIAN_POINT ( 'NONE',  ( 69.40000000109246514, 9.143825827087052716, 12.93301269999999192 ) ) ;
#6109 = VECTOR ( 'NONE', #20188, 999.9999999999998863 ) ;
#6110 = EDGE_CURVE ( 'NONE', #16229, #9984, #18261, .T. ) ;
#6111 = ORIENTED_EDGE ( 'NONE', *, *, #9687, .F. ) ;
#6112 = VECTOR ( 'NONE', #11849, 1000.000000000000000 ) ;
#6113 = CARTESIAN_POINT ( 'NONE',  ( 0.000000000000000000, 0.000000000000000000, 0.000000000000000000 ) ) ;
#6114 = CARTESIAN_POINT ( 'NONE',  ( -35.00000000000000711, 7.500000000000001776, -49.99999999999998579 ) ) ;
#6115 = CARTESIAN_POINT ( 'NONE',  ( 70.15000000109246514, 8.538419263543524096, 13.53841926354352054 ) ) ;
#6116 = CARTESIAN_POINT ( 'NONE',  ( -1.432654583217639610, -3.458734124999999882, 14.62500000136560629 ) ) ;
#6117 = PLANE ( 'NONE',  #931 ) ;
#6118 = CARTESIAN_POINT ( 'NONE',  ( 0.000000000000000000, 0.000000000000000000, 0.000000000000000000 ) ) ;
#6119 = STYLED_ITEM ( 'NONE', ( #19447 ), #22443 ) ;
#6120 = CARTESIAN_POINT ( 'NONE',  ( 4.000000000000000000, 1.656854249492381248, -0.1374999999999984013 ) ) ;
#6121 = CARTESIAN_POINT ( 'NONE',  ( -19.99999999999999645, -9.000000000000003553, 10.00000000000008882 ) ) ;
#6122 = CARTESIAN_POINT ( 'NONE',  ( 1.799999999999999600, 0.000000000000000000, -8.800000000000023803 ) ) ;
#6123 = B_SPLINE_CURVE_WITH_KNOTS ( 'NONE', 3,
 ( #21645, #23580, #12598, #20317, #19970, #14736 ),
 .UNSPECIFIED., .F., .F.,
 ( 4, 2, 4 ),
 ( 2.380733003329261875E-07, 0.001898835937927393497, 0.003797433802554454115 ),
 .UNSPECIFIED. ) ;
#6124 = CARTESIAN_POINT ( 'NONE',  ( 2.828427124746189847, 2.828427124746190291, -1.074999999999997735 ) ) ;
#6125 = EDGE_LOOP ( 'NONE', ( #17154, #4798, #14221, #5206 ) ) ;
#6126 = CARTESIAN_POINT ( 'NONE',  ( -67.00000000109247367, 12.06698729999999919, 14.14382582708705094 ) ) ;
#6127 = VERTEX_POINT ( 'NONE', #12337 ) ;
#6128 = CARTESIAN_POINT ( 'NONE',  ( 56.53125000000000711, 11.65685424949239923, 18.99999999999998934 ) ) ;
#6129 = CARTESIAN_POINT ( 'NONE',  ( -68.75000000109245946, 11.46158073645647235, 13.53841926354352232 ) ) ;
#6130 = PRODUCT_CONTEXT ( 'NONE', #7335, 'mechanical' ) ;
#6131 = B_SPLINE_CURVE_WITH_KNOTS ( 'NONE', 3,
 ( #8749, #21530, #6823, #21412, #6953, #2748, #22867, #6481, #13803, #8999, #3465, #16806, #12827, #19740, #12601, #21772 ),
 .UNSPECIFIED., .F., .F.,
 ( 4, 2, 2, 2, 2, 2, 2, 4 ),
 ( 0.000000000000000000, 0.001180799220441102609, 0.001771198830661654131, 0.002361598440882205219, 0.002951998051102756523, 0.003542397661323308262, 0.004132797271543859133, 0.004723196881764409570 ),
 .UNSPECIFIED. ) ;
#6132 = ORIENTED_EDGE ( 'NONE', *, *, #22768, .F. ) ;
#6133 = CARTESIAN_POINT ( 'NONE',  ( 44.10446624071656174, -8.974600000000002353, 10.00000000000008882 ) ) ;
#6134 = ORIENTED_EDGE ( 'NONE', *, *, #302, .F. ) ;
#6135 = VECTOR ( 'NONE', #21460, 1000.000000000000000 ) ;
#6136 = VECTOR ( 'NONE', #19441, 1000.000000000000114 ) ;
#6137 = EDGE_CURVE ( 'NONE', #9090, #7429, #1633, .T. ) ;
#6138 = EDGE_CURVE ( 'NONE', #16102, #22841, #12168, .T. ) ;
#6139 = ORIENTED_EDGE ( 'NONE', *, *, #174, .F. ) ;
#6140 = CARTESIAN_POINT ( 'NONE',  ( 1.872352939448454495E-15, -3.458734125000000770, 15.93750000136560629 ) ) ;
#6141 = CARTESIAN_POINT ( 'NONE',  ( 57.84375000000000711, 8.757359312880723223, 18.00000000000000355 ) ) ;
#6142 = VECTOR ( 'NONE', #16606, 1000.000000000000114 ) ;
#6143 = CARTESIAN_POINT ( 'NONE',  ( -66.60000000109248219, 7.933012699999995476, 15.85617417291294196 ) ) ;
#6144 = CIRCLE ( 'NONE', #15719, 2.649999999999989253 ) ;
#6145 = CARTESIAN_POINT ( 'NONE',  ( 67.55000000109247082, 8.538419263543524096, 13.53841926354352054 ) ) ;
#6146 = ADVANCED_FACE ( 'NONE', ( #16032 ), #12701, .F. ) ;
#6147 = CARTESIAN_POINT ( 'NONE',  ( -66.65000000109247935, 9.999999999999998224, 17.06698730000000097 ) ) ;
#6148 = DIRECTION ( 'NONE',  ( -1.000000000000000000, -0.000000000000000000, -0.000000000000000000 ) ) ;
#6149 = CARTESIAN_POINT ( 'NONE',  ( 56.87268183416158962, 7.926799079670491466, 12.83056023321021755 ) ) ;
#6150 = CARTESIAN_POINT ( 'NONE',  ( 60.00000000000001421, 12.34294812806585462, 13.10030744094656008 ) ) ;
#6151 = CARTESIAN_POINT ( 'NONE',  ( 6.353591512924457348E-16, -3.458734125000000770, 3.237500001365597679 ) ) ;
#6152 = LINE ( 'NONE', #394, #13198 ) ;
#6153 = CARTESIAN_POINT ( 'NONE',  ( 4.000000000000001776, -1.656854249492379694, 12.56250000273119660 ) ) ;
#6154 = CARTESIAN_POINT ( 'NONE',  ( 19.99999999999999645, 4.500000000000003553, -50.00000000000000000 ) ) ;
#6155 = CIRCLE ( 'NONE', #3716, 8.749000000000004107 ) ;
#6156 = ORIENTED_EDGE ( 'NONE', *, *, #13669, .T. ) ;
#6157 = CYLINDRICAL_SURFACE ( 'NONE', #3227, 4.000000000000000000 ) ;
#6158 = ORIENTED_EDGE ( 'NONE', *, *, #1321, .T. ) ;
#6159 = CARTESIAN_POINT ( 'NONE',  ( 60.71643183416158962, 12.97181229448535689, 16.31069182806490758 ) ) ;
#6160 = VECTOR ( 'NONE', #14149, 1000.000000000000000 ) ;
#6161 = CARTESIAN_POINT ( 'NONE',  ( 3.458734125000000326, 4.235727675282971730E-16, 3.237500001365597679 ) ) ;
#6162 = ADVANCED_FACE ( 'NONE', ( #1752 ), #21625, .T. ) ;
#6163 = CARTESIAN_POINT ( 'NONE',  ( 1.432654583217639832, 3.458734125000000326, 0.4250000013655961251 ) ) ;
#6164 = ORIENTED_EDGE ( 'NONE', *, *, #15403, .F. ) ;
#6165 = CARTESIAN_POINT ( 'NONE',  ( -2.828427124746188515, -2.828427124746190735, 14.12500000000001066 ) ) ;
#6166 = FILL_AREA_STYLE ('',( #11936 ) ) ;
#6167 = EDGE_CURVE ( 'NONE', #3575, #20722, #16733, .T. ) ;
#6168 = CARTESIAN_POINT ( 'NONE',  ( 2.500000000000000000, 1.178949249685212974, -2.042000000000001148 ) ) ;
#6169 = EDGE_LOOP ( 'NONE', ( #13713, #11260 ) ) ;
#6170 = CARTESIAN_POINT ( 'NONE',  ( -69.75000000218496155, 8.964466094067258695, 12.49999999999999289 ) ) ;
#6171 = EDGE_CURVE ( 'NONE', #1126, #6074, #5231, .T. ) ;
#6172 = DIRECTION ( 'NONE',  ( 1.000000000000000000, 0.000000000000000000, -1.224646799147353207E-16 ) ) ;
#6173 = VECTOR ( 'NONE', #16627, 1000.000000000000000 ) ;
#6174 = EDGE_CURVE ( 'NONE', #4148, #8748, #5650, .T. ) ;
#6175 = DIRECTION ( 'NONE',  ( -0.000000000000000000, -0.000000000000000000, 1.000000000000000000 ) ) ;
#6176 = CARTESIAN_POINT ( 'NONE',  ( 66.64999999999999147, 12.50000000000000000, 13.96446609406725869 ) ) ;
#6177 = DIRECTION ( 'NONE',  ( 1.000000000000000000, -0.000000000000000000, -0.000000000000000000 ) ) ;
#6178 = CARTESIAN_POINT ( 'NONE',  ( 68.70000000109246230, 12.06698730000000275, 15.85617417291294196 ) ) ;
#6179 = DIRECTION ( 'NONE',  ( 0.000000000000000000, -0.5877852522924802425, 0.8090169943749422332 ) ) ;
#6180 = CARTESIAN_POINT ( 'NONE',  ( 53.18981816583844591, 9.931948859054354983, 11.99999999999999645 ) ) ;
#6181 = CARTESIAN_POINT ( 'NONE',  ( 1.432654583217642275, -3.458734124999999437, -2.949999998634404985 ) ) ;
#6182 = CARTESIAN_POINT ( 'NONE',  ( 2.445694354108821411, 2.445694354108820523, 12.31250000136560629 ) ) ;
#6183 = DIRECTION ( 'NONE',  ( -7.087422195345011518E-32, -1.000000000000000000, -0.000000000000000000 ) ) ;
#6184 = CARTESIAN_POINT ( 'NONE',  ( -71.00000000109247367, 9.143825827087052716, 12.93301269999999192 ) ) ;
#6185 = CARTESIAN_POINT ( 'NONE',  ( 65.55000000218494449, 7.499999999999996447, 16.03553390593273775 ) ) ;
#6186 = EDGE_LOOP ( 'NONE', ( #6139, #23582, #17119, #9460, #19176, #1721, #22587 ) ) ;
#6187 = DIRECTION ( 'NONE',  ( 1.000000000000000000, -0.000000000000000000, 0.000000000000000000 ) ) ;
#6188 = CARTESIAN_POINT ( 'NONE',  ( 1.656854249492380360, 4.000000000000000000, 3.112500002731188875 ) ) ;
#6189 = CARTESIAN_POINT ( 'NONE',  ( -70.10000000109246798, 10.85617417291294551, 12.93301269999999370 ) ) ;
#6190 = ORIENTED_EDGE ( 'NONE', *, *, #13667, .F. ) ;
#6191 = ORIENTED_EDGE ( 'NONE', *, *, #19908, .F. ) ;
#6192 = DIRECTION ( 'NONE',  ( -1.000000000000000000, 0.000000000000000000, 0.000000000000000000 ) ) ;
#6193 = ADVANCED_BREP_SHAPE_REPRESENTATION ( '', ( #22443, #7318 ), #16773 ) ;
#6194 = CARTESIAN_POINT ( 'NONE',  ( 51.46875000000000711, 5.999999999999987566, 13.34314575050763452 ) ) ;
#6195 = VERTEX_POINT ( 'NONE', #19835 ) ;
#6196 = CARTESIAN_POINT ( 'NONE',  ( 4.999999999999999112, -4.729683950898817102, -7.360373001730970977 ) ) ;
#6197 = UNCERTAINTY_MEASURE_WITH_UNIT (LENGTH_MEASURE( 1.000000000000000082E-05 ), #6630, 'distance_accuracy_value', 'NONE');
#6198 = EDGE_CURVE ( 'NONE', #14695, #5303, #11124, .T. ) ;
#6199 = CARTESIAN_POINT ( 'NONE',  ( 67.60000000109248219, 9.143825827087050939, 12.93301269999999370 ) ) ;
#6200 = EDGE_CURVE ( 'NONE', #20722, #3223, #9879, .T. ) ;
#6201 = CARTESIAN_POINT ( 'NONE',  ( 68.55000000109247082, 8.538419263543524096, 13.53841926354352054 ) ) ;
#6202 = ORIENTED_EDGE ( 'NONE', *, *, #7337, .F. ) ;
#6203 = DIRECTION ( 'NONE',  ( -1.000000000000000000, -7.703719777548943412E-32, 0.000000000000000000 ) ) ;
#6204 = CARTESIAN_POINT ( 'NONE',  ( 57.00000000000000000, 12.82842712474617741, 12.17157287525379239 ) ) ;
#6205 = CARTESIAN_POINT ( 'NONE',  ( -2.828427124746188515, -2.828427124746190735, 12.25000000273119838 ) ) ;
#6206 = CYLINDRICAL_SURFACE ( 'NONE', #2838, 2.500000000000002220 ) ;
#6207 = CARTESIAN_POINT ( 'NONE',  ( 51.00000000000000711, 12.47487373415290612, 12.52512626584706901 ) ) ;
#6208 = DIRECTION ( 'NONE',  ( -1.000000000000000000, 0.000000000000000000, 0.000000000000000000 ) ) ;
#6209 = ORIENTED_EDGE ( 'NONE', *, *, #12561, .T. ) ;
#6210 = CARTESIAN_POINT ( 'NONE',  ( -54.99999999999992895, 15.00000000000000000, 1.387778780781445676E-14 ) ) ;
#6211 = CARTESIAN_POINT ( 'NONE',  ( -4.000000000000000000, 0.000000000000000000, -3.574999997268813345 ) ) ;
#6212 = CARTESIAN_POINT ( 'NONE',  ( 4.999999999999999112, -1.239665997526817165, -9.314797388894906049 ) ) ;
#6213 = EDGE_LOOP ( 'NONE', ( #7351, #18786, #14606, #6611 ) ) ;
#6214 = DIRECTION ( 'NONE',  ( 0.000000000000000000, 0.000000000000000000, -1.000000000000000000 ) ) ;
#6215 = FACE_BOUND ( 'NONE', #2902, .T. ) ;
#6216 = LINE ( 'NONE', #22725, #13254 ) ;
#6217 = AXIS2_PLACEMENT_3D ( 'NONE', #11627, #7896, #8019 ) ;
#6218 = CARTESIAN_POINT ( 'NONE',  ( 40.96287359071656908, -8.974600000000002353, 10.00000000000008882 ) ) ;
#6219 = EDGE_LOOP ( 'NONE', ( #2871, #15284, #6438, #909 ) ) ;
#6220 = CARTESIAN_POINT ( 'NONE',  ( 0.5316568767328664347, 7.198601258566900363, -0.4033376246892524941 ) ) ;
#6221 = VERTEX_POINT ( 'NONE', #11000 ) ;
#6222 = CARTESIAN_POINT ( 'NONE',  ( 70.90000000109247935, 10.85617417291294551, 12.93301269999999192 ) ) ;
#6223 =( BOUNDED_CURVE ( )  B_SPLINE_CURVE ( 2, ( #12562, #23662, #16018, #12794, #7151, #12435, #5458, #21851, #10876 ),
 .UNSPECIFIED., .F., .F. ) 
 B_SPLINE_CURVE_WITH_KNOTS ( ( 3, 2, 2, 2, 3 ),
 ( 0.4374999999999995004, 0.4531249999999993894, 0.4687499999999993339, 0.4843749999999992228, 0.4999999999999991118 ),
 .UNSPECIFIED. ) 
 CURVE ( )  GEOMETRIC_REPRESENTATION_ITEM ( )  RATIONAL_B_SPLINE_CURVE ( ( 1.000000000000002442, 0.9238795325112842960, 1.000000000000000000, 0.9238795325112867385, 1.000000000000000000, 0.9238795325112867385, 1.000000000000000000, 0.9238795325112910684, 0.9999999999999956701 ) ) 
 REPRESENTATION_ITEM ( '' )  );
#6224 = CARTESIAN_POINT ( 'NONE',  ( 1.971781867644420635E-15, -4.000000000000000000, 11.25000000000001066 ) ) ;
#6225 = DIRECTION ( 'NONE',  ( -1.000000000000000000, 0.000000000000000000, -0.000000000000000000 ) ) ;
#6226 = CARTESIAN_POINT ( 'NONE',  ( 1.067197363239223984, 6.889406814520512512, -3.442664554191215753 ) ) ;
#6227 = DIRECTION ( 'NONE',  ( 0.000000000000000000, 0.000000000000000000, -1.000000000000000000 ) ) ;
#6228 = CARTESIAN_POINT ( 'NONE',  ( 71.05000000109245661, 9.999999999999998224, 12.93301269999999192 ) ) ;
#6229 = ORIENTED_EDGE ( 'NONE', *, *, #8109, .F. ) ;
#6230 = CARTESIAN_POINT ( 'NONE',  ( 4.000000000000000000, 4.898587196589412829E-16, 0.9250000027311873207 ) ) ;
#6231 = PLANE ( 'NONE',  #15673 ) ;
#6232 = CARTESIAN_POINT ( 'NONE',  ( 69.25000000109245946, 7.933012699999995476, 14.99999999999999645 ) ) ;
#6233 = CARTESIAN_POINT ( 'NONE',  ( -1.432654583217638944, 3.458734125000000326, 12.25000000136560452 ) ) ;
#6234 = DIRECTION ( 'NONE',  ( 0.000000000000000000, 0.000000000000000000, -1.000000000000000000 ) ) ;
#6235 = ADVANCED_FACE ( 'NONE', ( #3782 ), #10642, .T. ) ;
#6236 = DIRECTION ( 'NONE',  ( 0.000000000000000000, 0.000000000000000000, 1.000000000000000000 ) ) ;
#6237 = ORIENTED_EDGE ( 'NONE', *, *, #14071, .T. ) ;
#6238 = CARTESIAN_POINT ( 'NONE',  ( -2.449293598294706907E-16, 4.000000000000000000, 0.05000000000000143219 ) ) ;
#6239 = LINE ( 'NONE', #835, #10955 ) ;
#6240 = CARTESIAN_POINT ( 'NONE',  ( -2.445694354108818303, -2.445694354108820523, 10.56250000136560452 ) ) ;
#6241 = CARTESIAN_POINT ( 'NONE',  ( -65.00000000000000000, 15.00000000000000000, 10.00000000000008882 ) ) ;
#6242 = MANIFOLD_SOLID_BREP ( 'Hex', #11643 ) ;
#6243 = EDGE_LOOP ( 'NONE', ( #11239, #16584, #4919, #18935 ) ) ;
#6244 = CARTESIAN_POINT ( 'NONE',  ( -67.25000000109247367, 9.999999999999998224, 17.06698730000000097 ) ) ;
#6245 = ORIENTED_EDGE ( 'NONE', *, *, #7610, .T. ) ;
#6246 = CARTESIAN_POINT ( 'NONE',  ( -66.65000000109247935, 9.999999999999998224, 17.06698730000000097 ) ) ;
#6247 = ITEM_DEFINED_TRANSFORMATION ( 'NONE', 'NONE', #8803,  #7318 ) ;
#6248 = ORIENTED_EDGE ( 'NONE', *, *, #7341, .F. ) ;
#6249 = LINE ( 'NONE', #22759, #5954 ) ;
#6250 = ORIENTED_EDGE ( 'NONE', *, *, #8109, .T. ) ;
#6251 = ORIENTED_EDGE ( 'NONE', *, *, #19640, .F. ) ;
#6252 = CARTESIAN_POINT ( 'NONE',  ( -1.432654583217639166, 3.458734125000000770, 16.50000000136560629 ) ) ;
#6253 = CARTESIAN_POINT ( 'NONE',  ( 0.000000000000000000, 7.958834565716766285, 7.593217523260609170 ) ) ;
#6254 = AXIS2_PLACEMENT_3D ( 'NONE', #3923, #19105, #13619 ) ;
#6255 = CARTESIAN_POINT ( 'NONE',  ( -69.10000000109248219, 7.933012699999995476, 14.14382582708705094 ) ) ;
#6256 = CIRCLE ( 'NONE', #19621, 6.735000000000022524 ) ;
#6257 = CARTESIAN_POINT ( 'NONE',  ( 67.85000000109248219, 12.06698730000000097, 14.99999999999999645 ) ) ;
#6258 = CARTESIAN_POINT ( 'NONE',  ( -68.15000000109246514, 11.46158073645647235, 16.46158073645647235 ) ) ;
#6259 = VECTOR ( 'NONE', #20213, 1000.000000000000000 ) ;
#6260 = FACE_OUTER_BOUND ( 'NONE', #7015, .T. ) ;
#6261 = CARTESIAN_POINT ( 'NONE',  ( 59.31018183416157541, 12.99999999999999822, 15.06805114094562192 ) ) ;
#6262 = CARTESIAN_POINT ( 'NONE',  ( 45.00000000000000000, 10.00000000000001599, 17.50000000000003197 ) ) ;
#6263 = EDGE_CURVE ( 'NONE', #8909, #660, #13153, .T. ) ;
#6264 = CLOSED_SHELL ( 'NONE', ( #7600, #1733, #21363, #9358, #19344, #17870, #14789, #19776, #14472, #21696, #15928, #10706, #16813, #7027, #14271, #20031, #9165, #708, #10005, #11588, #20368, #18739, #17383, #752, #9003, #18263, #142, #6235, #2204, #6997, #13643, #2277, #9274, #9664, #8621, #22119, #19165, #22942, #11576, #10376, #612, #11297, #5596, #19605 ) ) ;
#6265 = CARTESIAN_POINT ( 'NONE',  ( -3.458734125000000326, -1.432654583217642497, 3.050000001365598568 ) ) ;
#6266 = EDGE_CURVE ( 'NONE', #1904, #13424, #15192, .T. ) ;
#6267 = LINE ( 'NONE', #12143, #22721 ) ;
#6268 = CARTESIAN_POINT ( 'NONE',  ( 4.000000000000000888, 1.656854249492381248, 10.68750000273119483 ) ) ;
#6269 = DIRECTION ( 'NONE',  ( -1.000000000000000000, 0.000000000000000000, -0.000000000000000000 ) ) ;
#6270 = AXIS2_PLACEMENT_3D ( 'NONE', #7624, #18617, #2206 ) ;
#6271 = ORIENTED_EDGE ( 'NONE', *, *, #21288, .F. ) ;
#6272 = PLANE ( 'NONE',  #21188 ) ;
#6273 = ORIENTED_EDGE ( 'NONE', *, *, #1462, .F. ) ;
#6274 = CARTESIAN_POINT ( 'NONE',  ( 60.15393183416158962, 6.971812294485357775, 16.17458954617365663 ) ) ;
#6275 = CARTESIAN_POINT ( 'NONE',  ( 0.000000000000000000, 0.000000000000000000, 0.000000000000000000 ) ) ;
#6276 = CARTESIAN_POINT ( 'NONE',  ( 2.445694354108820079, 2.445694354108820523, 0.3625000013655951259 ) ) ;
#6277 = EDGE_CURVE ( 'NONE', #4086, #22517, #7407, .T. ) ;
#6278 = CARTESIAN_POINT ( 'NONE',  ( -2.445694354108819635, -2.445694354108820523, 1.862500001365596347 ) ) ;
#6279 = ORIENTED_EDGE ( 'NONE', *, *, #1739, .T. ) ;
#6280 = B_SPLINE_CURVE_WITH_KNOTS ( 'NONE', 3,
 ( #22246, #5744, #7435, #14748, #13072, #5856, #2727, #17243 ),
 .UNSPECIFIED., .F., .F.,
 ( 4, 2, 2, 4 ),
 ( 2.465131517075058656E-07, 0.001183067374689851080, 0.001774477805458923299, 0.002365888236227995517 ),
 .UNSPECIFIED. ) ;
#6281 = CARTESIAN_POINT ( 'NONE',  ( -2.828427124746189403, 2.828427124746190291, 13.87500000000001066 ) ) ;
#6282 = FACE_OUTER_BOUND ( 'NONE', #16351, .T. ) ;
#6283 = CARTESIAN_POINT ( 'NONE',  ( -6.161016159283438931, -8.974600000000002353, 5.000000000000079936 ) ) ;
#6284 = ORIENTED_EDGE ( 'NONE', *, *, #11791, .F. ) ;
#6285 = CARTESIAN_POINT ( 'NONE',  ( -70.15000000218495302, 11.03553390593273598, 17.50000000000000355 ) ) ;
#6286 = CARTESIAN_POINT ( 'NONE',  ( -3.458734125000000770, 1.432654583217640498, -2.074999998634404097 ) ) ;
#6287 = LINE ( 'NONE', #20869, #2626 ) ;
#6288 = DIRECTION ( 'NONE',  ( 0.000000000000000000, 0.8090169943749487835, -0.5877852522924714718 ) ) ;
#6289 = ADVANCED_FACE ( 'NONE', ( #13040 ), #7759, .F. ) ;
#6290 = AXIS2_PLACEMENT_3D ( 'NONE', #20965, #19188, #19410 ) ;
#6291 = DIRECTION ( 'NONE',  ( 0.000000000000000000, 0.000000000000000000, 1.000000000000000000 ) ) ;
#6292 = CARTESIAN_POINT ( 'NONE',  ( 68.55000000109247082, 11.46158073645647235, 13.53841926354352232 ) ) ;
#6293 = ADVANCED_FACE ( 'NONE', ( #9679 ), #22092, .F. ) ;
#6294 = DIRECTION ( 'NONE',  ( -1.000000000000000000, -0.000000000000000000, -0.000000000000000000 ) ) ;
#6295 = CARTESIAN_POINT ( 'NONE',  ( 54.78356816583844591, 8.689308171935074654, 12.02818770551464489 ) ) ;
#6296 = EDGE_CURVE ( 'NONE', #611, #22180, #16728, .T. ) ;
#6297 = CARTESIAN_POINT ( 'NONE',  ( -2.117863837641485618E-16, 3.458734125000000326, -3.512499998634403209 ) ) ;
#6298 = CARTESIAN_POINT ( 'NONE',  ( -3.458734124999999437, 0.000000000000000000, 11.68750000136560629 ) ) ;
#6299 = DIRECTION ( 'NONE',  ( -0.000000000000000000, -0.000000000000000000, 1.000000000000000000 ) ) ;
#6300 = CARTESIAN_POINT ( 'NONE',  ( -68.15000000109246514, 11.46158073645647235, 16.46158073645647235 ) ) ;
#6301 = CARTESIAN_POINT ( 'NONE',  ( -70.00000000218494733, 12.50000000000000000, 14.99999999999999645 ) ) ;
#6302 = CARTESIAN_POINT ( 'NONE',  ( 8.673617379884035472E-16, 7.505553499465136724, -3.700000000000000178 ) ) ;
#6303 = ORIENTED_EDGE ( 'NONE', *, *, #1393, .T. ) ;
#6304 = CARTESIAN_POINT ( 'NONE',  ( -1.257172072275743346, 3.892973519171203378, -3.433252694550776862 ) ) ;
#6305 = VECTOR ( 'NONE', #21470, 1000.000000000000000 ) ;
#6306 = SHAPE_REPRESENTATION_RELATIONSHIP ( 'NONE' , 'NONE' ,  #13579, #5892 ) ;
#6307 = CARTESIAN_POINT ( 'NONE',  ( -4.000000000000000888, 1.656854249492380804, 5.362500002731188431 ) ) ;
#6308 = EDGE_CURVE ( 'NONE', #4290, #14520, #18402, .T. ) ;
#6309 = ORIENTED_EDGE ( 'NONE', *, *, #2197, .T. ) ;
#6310 = EDGE_CURVE ( 'NONE', #2142, #9984, #20910, .T. ) ;
#6311 = VERTEX_POINT ( 'NONE', #16611 ) ;
#6312 = CARTESIAN_POINT ( 'NONE',  ( 4.999999999999999112, 9.241976615262160522, 2.300561732649595736 ) ) ;
#6313 = LINE ( 'NONE', #7997, #20157 ) ;
#6314 = VERTEX_POINT ( 'NONE', #15077 ) ;
#6315 = CARTESIAN_POINT ( 'NONE',  ( 11.86036186966726191, -11.25000000000000355, 5.000000000000079936 ) ) ;
#6316 = CARTESIAN_POINT ( 'NONE',  ( 67.30000000109247082, 9.143825827087049163, 17.06698729999999742 ) ) ;
#6317 = VECTOR ( 'NONE', #14477, 1000.000000000000000 ) ;
#6318 = AXIS2_PLACEMENT_3D ( 'NONE', #5327, #3409, #12779 ) ;
#6319 = CARTESIAN_POINT ( 'NONE',  ( 69.30000000109247082, 7.933012699999995476, 14.14382582708705094 ) ) ;
#6320 = VECTOR ( 'NONE', #6593, 1000.000000000000000 ) ;
#6321 = ORIENTED_EDGE ( 'NONE', *, *, #6055, .T. ) ;
#6322 = FACE_OUTER_BOUND ( 'NONE', #12369, .T. ) ;
#6323 = CARTESIAN_POINT ( 'NONE',  ( 54.75000000000000711, 7.171572875253819923, 17.82842712474619873 ) ) ;
#6324 = EDGE_CURVE ( 'NONE', #3286, #10092, #190, .T. ) ;
#6325 = DIRECTION ( 'NONE',  ( 0.000000000000000000, 0.000000000000000000, 1.000000000000000000 ) ) ;
#6326 = CARTESIAN_POINT ( 'NONE',  ( 3.458734125000001214, 4.235727675282971730E-16, 18.93750000136560629 ) ) ;
#6327 = CYLINDRICAL_SURFACE ( 'NONE', #10570, 11.00000000000000000 ) ;
#6328 = DIRECTION ( 'NONE',  ( 0.000000000000000000, 0.000000000000000000, -1.000000000000000000 ) ) ;
#6329 = ORIENTED_EDGE ( 'NONE', *, *, #5067, .T. ) ;
#6330 = CARTESIAN_POINT ( 'NONE',  ( 1.799999999999999156, 0.000000000000000000, 0.000000000000000000 ) ) ;
#6331 = EDGE_CURVE ( 'NONE', #11486, #1543, #6412, .T. ) ;
#6332 = CARTESIAN_POINT ( 'NONE',  ( 29.00211400323381028, -9.000000000000005329, 5.000000000000079936 ) ) ;
#6333 = CARTESIAN_POINT ( 'NONE',  ( -70.50000000000000000, 9.999999999999998224, 12.49999999999999289 ) ) ;
#6334 = ADVANCED_FACE ( 'NONE', ( #22941, #11607, #10045 ), #23054, .T. ) ;
#6335 = ORIENTED_EDGE ( 'NONE', *, *, #6171, .T. ) ;
#6336 = DIRECTION ( 'NONE',  ( -0.000000000000000000, -1.000000000000000000, 0.000000000000000000 ) ) ;
#6337 = DIRECTION ( 'NONE',  ( -1.000000000000000000, 0.000000000000000000, 1.224646799147353207E-16 ) ) ;
#6338 = CARTESIAN_POINT ( 'NONE',  ( -4.000000000000000000, 0.000000000000000000, -0.5749999972688123462 ) ) ;
#6339 = CIRCLE ( 'NONE', #18956, 5.000000000000000888 ) ;
#6340 = CIRCLE ( 'NONE', #21608, 4.000000000000002665 ) ;
#6341 = CARTESIAN_POINT ( 'NONE',  ( 1.236993788156008760E-15, 0.000000000000000000, 21.31370849898476649 ) ) ;
#6342 = ORIENTED_EDGE ( 'NONE', *, *, #18614, .F. ) ;
#6343 = CARTESIAN_POINT ( 'NONE',  ( -68.60000000218495586, 9.999999999999998224, 17.49999999999999645 ) ) ;
#6344 = ORIENTED_EDGE ( 'NONE', *, *, #21389, .F. ) ;
#6345 = CARTESIAN_POINT ( 'NONE',  ( 4.000000000000000888, 4.898587196589412829E-16, 17.50000000000001066 ) ) ;
#6346 = CARTESIAN_POINT ( 'NONE',  ( -1.647987302177966740E-14, -7.505553499465137612, -3.119443416399232394 ) ) ;
#6347 = CARTESIAN_POINT ( 'NONE',  ( 70.10000000218494165, 11.76776695296636888, 16.76776695296636532 ) ) ;
#6348 = CARTESIAN_POINT ( 'NONE',  ( -3.999999999999998224, -1.656854249492383024, 19.06250000000001421 ) ) ;
#6349 = CARTESIAN_POINT ( 'NONE',  ( -4.000000000000000000, 2.309401076758498483, -0.4999999999999927280 ) ) ;
#6350 = CARTESIAN_POINT ( 'NONE',  ( 66.80000000109247082, 7.933012699999995476, 15.85617417291294196 ) ) ;
#6351 = ORIENTED_EDGE ( 'NONE', *, *, #3664, .T. ) ;
#6352 = AXIS2_PLACEMENT_3D ( 'NONE', #17632, #21179, #5037 ) ;
#6353 = DIRECTION ( 'NONE',  ( 0.000000000000000000, 0.000000000000000000, -1.000000000000000000 ) ) ;
#6354 = AXIS2_PLACEMENT_3D ( 'NONE', #12799, #12330, #16372 ) ;
#6355 = CARTESIAN_POINT ( 'NONE',  ( 4.999999999999999112, 8.264486777890107660, 4.472189673936815879 ) ) ;
#6356 = CARTESIAN_POINT ( 'NONE',  ( 69.35000000109246798, 8.538419263543524096, 13.53841926354352054 ) ) ;
#6357 = CARTESIAN_POINT ( 'NONE',  ( 1.872352939448454495E-15, -3.458734125000000326, 14.68750000136560452 ) ) ;
#6358 = DIRECTION ( 'NONE',  ( -6.974779929323510821E-32, -1.000000000000000000, 5.754033390038005467E-16 ) ) ;
#6359 = DIRECTION ( 'NONE',  ( 0.000000000000000000, 0.000000000000000000, -1.000000000000000000 ) ) ;
#6360 = ORIENTED_EDGE ( 'NONE', *, *, #19192, .T. ) ;
#6361 = CARTESIAN_POINT ( 'NONE',  ( -4.000000000000000888, 1.656854249492380804, 3.237500000000002931 ) ) ;
#6362 = CARTESIAN_POINT ( 'NONE',  ( -19.99999999999999645, -9.000000000000003553, 5.000000000000079936 ) ) ;
#6363 = CARTESIAN_POINT ( 'NONE',  ( 4.000000000000000000, 4.898587196589412829E-16, -0.07499999726881187434 ) ) ;
#6364 = CARTESIAN_POINT ( 'NONE',  ( -4.000000000000000000, 0.000000000000000000, -0.6999999999999975131 ) ) ;
#6365 = EDGE_CURVE ( 'NONE', #9347, #14277, #14078, .T. ) ;
#6366 = ORIENTED_EDGE ( 'NONE', *, *, #5865, .F. ) ;
#6367 = CARTESIAN_POINT ( 'NONE',  ( 18.96248019676620444, -9.000000000000005329, 5.000000000000079936 ) ) ;
#6368 = ORIENTED_EDGE ( 'NONE', *, *, #15144, .T. ) ;
#6369 = CARTESIAN_POINT ( 'NONE',  ( -68.25000000109245946, 9.999999999999998224, 17.06698730000000097 ) ) ;
#6370 =( BOUNDED_CURVE ( )  B_SPLINE_CURVE ( 2, ( #2291, #3722, #376, #20486, #5417, #20007, #22279, #4087, #14782 ),
 .UNSPECIFIED., .F., .F. ) 
 B_SPLINE_CURVE_WITH_KNOTS ( ( 3, 2, 2, 2, 3 ),
 ( 0.4000000000000000222, 0.4124999999999999778, 0.4249999999999999889, 0.4375000000000000000, 0.4500000000000000111 ),
 .UNSPECIFIED. ) 
 CURVE ( )  GEOMETRIC_REPRESENTATION_ITEM ( )  RATIONAL_B_SPLINE_CURVE ( ( 1.000000000000000000, 0.9238795325112867385, 1.000000000000000000, 0.9238795325112867385, 1.000000000000000000, 0.9238795325112867385, 1.000000000000000000, 0.9238795325112867385, 1.000000000000000000 ) ) 
 REPRESENTATION_ITEM ( '' )  );
#6371 = ORIENTED_EDGE ( 'NONE', *, *, #10275, .T. ) ;
#6372 = DIRECTION ( 'NONE',  ( -1.000000000000000000, -0.000000000000000000, -0.000000000000000000 ) ) ;
#6373 = ORIENTED_EDGE ( 'NONE', *, *, #13376, .F. ) ;
#6374 = VERTEX_POINT ( 'NONE', #4270 ) ;
#6375 = CARTESIAN_POINT ( 'NONE',  ( 3.458734125000002546, -1.432654583217639610, 14.12500000136560452 ) ) ;
#6376 = CARTESIAN_POINT ( 'NONE',  ( 52.50000000000000711, 12.12132034355963484, 12.87867965644034740 ) ) ;
#6377 = CARTESIAN_POINT ( 'NONE',  ( -67.80000000109247082, 12.06698730000000275, 14.14382582708705094 ) ) ;
#6378 = CARTESIAN_POINT ( 'NONE',  ( 66.75000000109247367, 8.538419263543524096, 13.53841926354352054 ) ) ;
#6379 = CARTESIAN_POINT ( 'NONE',  ( -65.85000000109246798, 9.999999999999998224, 17.06698730000000097 ) ) ;
#6380 = LINE ( 'NONE', #13697, #19446 ) ;
#6381 = CARTESIAN_POINT ( 'NONE',  ( 54.99768183416157541, 12.16943976678977535, 12.92679907967048614 ) ) ;
#6382 = LINE ( 'NONE', #20849, #22683 ) ;
#6383 = CARTESIAN_POINT ( 'NONE',  ( 1.432654583217640276, 3.458734125000000770, 4.675000001365594571 ) ) ;
#6384 = CARTESIAN_POINT ( 'NONE',  ( -35.00000000000000711, 4.500000000000003553, -49.99999999999999289 ) ) ;
#6385 = CARTESIAN_POINT ( 'NONE',  ( -2.828427124746188515, -2.828427124746190735, 12.25000000273119838 ) ) ;
#6386 = FACE_BOUND ( 'NONE', #15366, .T. ) ;
#6387 = ORIENTED_EDGE ( 'NONE', *, *, #10242, .T. ) ;
#6388 = ORIENTED_EDGE ( 'NONE', *, *, #5688, .T. ) ;
#6389 = CARTESIAN_POINT ( 'NONE',  ( 57.62268183416157541, 12.07320092032950676, 17.16943976678977180 ) ) ;
#6390 = DIRECTION ( 'NONE',  ( 1.000000000000000000, 0.000000000000000000, 0.000000000000000000 ) ) ;
#6391 = CARTESIAN_POINT ( 'NONE',  ( -1.432654583217640942, -3.458734124999999882, 1.925000001365597457 ) ) ;
#6392 = CARTESIAN_POINT ( 'NONE',  ( -3.458734125000000326, 0.000000000000000000, -1.262499998634402765 ) ) ;
#6393 = VERTEX_POINT ( 'NONE', #20888 ) ;
#6394 = DIRECTION ( 'NONE',  ( -1.000000000000000000, -0.000000000000000000, -0.000000000000000000 ) ) ;
#6395 = CARTESIAN_POINT ( 'NONE',  ( 0.000000000000000000, -7.958834565716711218, -7.593217523260672230 ) ) ;
#6396 = B_SPLINE_CURVE_WITH_KNOTS ( 'NONE', 3,
 ( #19519, #11271, #7204, #16530, #9353, #3936 ),
 .UNSPECIFIED., .F., .F.,
 ( 4, 2, 4 ),
 ( 0.002365888236227995517, 0.003551327329835084114, 0.004736766423442172712 ),
 .UNSPECIFIED. ) ;
#6397 = VERTEX_POINT ( 'NONE', #6553 ) ;
#6398 = CARTESIAN_POINT ( 'NONE',  ( 9.920644283265380691E-16, 4.000000000000000000, 19.75000000000001066 ) ) ;
#6399 = ORIENTED_EDGE ( 'NONE', *, *, #6001, .T. ) ;
#6400 = CARTESIAN_POINT ( 'NONE',  ( 58.25231816583843170, 7.926799079670502124, 17.16943976678978245 ) ) ;
#6401 =( BOUNDED_CURVE ( )  B_SPLINE_CURVE ( 2, ( #10056, #15332, #1031, #15684, #19239, #9809, #20793, #562, #6326, #22714, #22830, #11737, #913, #22602, #676, #19000, #21024, #6444, #20903, #803, #9934, #22957, #4285, #8136, #11853, #4516, #19129, #2474, #6565, #22470, #2715, #17346, #7887, #9694, #10176, #13881, #15447, #21139, #18781, #2362, #15206, #6081, #5107, #23547, #19477, #8848, #14238, #12205, #19703, #5221, #7036, #3432, #17585, #12566, #1150, #3075, #10650, #14353, #6792, #1377, #15795, #12439, #6678, #8715, #3307, #4998, #17698, #1509, #10418, #8491, #10531, #19589, #17925, #12327, #13991, #23067, #21253, #14113, #10773, #16258, #1624, #21614, #23311, #1259, #16022, #19825, #3185, #21495, #16143, #4752, #4870, #23429, #7155, #18047, #12088, #8967, #14469, #8598, #19353, #2942, #15904, #23181, #6920, #10295, #21376, #17809, #7833, #15273, #9875, #19945, #20378, #2057, #3544, #12690, #6026, #263, #18719, #20622, #22295, #11324, #18835, #2534, #17170, #16690, #10880, #3984, #15154, #7601, #14920, #11446, #22415, #18949, #20501, #11568, #22544, #16934, #18597, #7953, #625, #18158, #9519, #9752, #2310, #21735, #9399, #2180, #510, #4229, #9643 ),
 .UNSPECIFIED., .F., .F. ) 
 B_SPLINE_CURVE_WITH_KNOTS ( ( 3, 2, 2, 2, 2, 2, 2, 2, 2, 2, 2, 2, 2, 2, 2, 2, 2, 2, 2, 2, 2, 2, 2, 2, 2, 2, 2, 2, 2, 2, 2, 2, 2, 2, 2, 2, 2, 2, 2, 2, 2, 2, 2, 2, 2, 2, 2, 2, 2, 2, 2, 2, 2, 2, 2, 2, 2, 2, 2, 2, 2, 2, 2, 2, 2, 2, 2, 2, 2, 2, 2, 2, 2, 2, 3 ),
 ( 0.000000000000000000, 0.01250000000000000069, 0.02500000000000000139, 0.03749999999999999861, 0.05000000000000000278, 0.06250000000000000000, 0.07499999999999999722, 0.08749999999999999445, 0.1000000000000000056, 0.1125000000000000028, 0.1250000000000000000, 0.1375000000000000111, 0.1499999999999999944, 0.1625000000000000056, 0.1749999999999999889, 0.1875000000000000278, 0.2000000000000000111, 0.2124999999999999944, 0.2250000000000000056, 0.2374999999999999889, 0.2500000000000000000, 0.2625000000000000111, 0.2750000000000000222, 0.2874999999999999778, 0.2999999999999999889, 0.3125000000000000000, 0.3250000000000000111, 0.3375000000000000777, 0.3499999999999999778, 0.3624999999999999889, 0.3750000000000000555, 0.3875000000000000111, 0.4000000000000000222, 0.4124999999999999223, 0.4249999999999999889, 0.4375000000000000000, 0.4500000000000000111, 0.4625000000000000222, 0.4749999999999999778, 0.4874999999999999889, 0.5000000000000000000, 0.5124999999999999556, 0.5250000000000000222, 0.5374999999999999778, 0.5500000000000000444, 0.5625000000000000000, 0.5749999999999999556, 0.5875000000000000222, 0.5999999999999999778, 0.6125000000000000444, 0.6250000000000000000, 0.6374999999999999556, 0.6500000000000000222, 0.6624999999999999778, 0.6750000000000001554, 0.6875000000000000000, 0.6999999999999999556, 0.7125000000000001332, 0.7249999999999999778, 0.7375000000000000444, 0.7500000000000001110, 0.7624999999999999556, 0.7750000000000000222, 0.7874999999999998668, 0.8000000000000000444, 0.8125000000000000000, 0.8249999999999998446, 0.8375000000000000222, 0.8499999999999999778, 0.8625000000000000444, 0.8750000000000000000, 0.8874999999999999556, 0.9000000000000000222, 0.9124999999999999778, 0.9250000000000000444 ),
 .UNSPECIFIED. ) 
 CURVE ( )  GEOMETRIC_REPRESENTATION_ITEM ( )  RATIONAL_B_SPLINE_CURVE ( ( 1.000000000000000000, 0.9238795325112867385, 1.000000000000000000, 0.9238795325112867385, 1.000000000000000000, 0.9238795325112867385, 1.000000000000000000, 0.9238795325112867385, 1.000000000000000000, 0.9238795325112867385, 1.000000000000000000, 0.9238795325112867385, 1.000000000000000000, 0.9238795325112867385, 1.000000000000000000, 0.9238795325112867385, 1.000000000000000000, 0.9238795325112867385, 1.000000000000000000, 0.9238795325112867385, 1.000000000000000000, 0.9238795325112867385, 1.000000000000000000, 0.9238795325112867385, 1.000000000000000000, 0.9238795325112867385, 1.000000000000000000, 0.9238795325112867385, 1.000000000000000000, 0.9238795325112867385, 1.000000000000000000, 0.9238795325112867385, 1.000000000000000000, 0.9238795325112867385, 1.000000000000000000, 0.9238795325112867385, 1.000000000000000000, 0.9238795325112867385, 1.000000000000000000, 0.9238795325112867385, 1.000000000000000000, 0.9238795325112867385, 1.000000000000000000, 0.9238795325112867385, 1.000000000000000000, 0.9238795325112867385, 1.000000000000000000, 0.9238795325112867385, 1.000000000000000000, 0.9238795325112867385, 1.000000000000000000, 0.9238795325112867385, 1.000000000000000000, 0.9238795325112867385, 1.000000000000000000, 0.9238795325112867385, 1.000000000000000000, 0.9238795325112867385, 1.000000000000000000, 0.9238795325112867385, 1.000000000000000000, 0.9238795325112867385, 1.000000000000000000, 0.9238795325112867385, 1.000000000000000000, 0.9238795325112867385, 1.000000000000000000, 0.9238795325112867385, 1.000000000000000000, 0.9238795325112867385, 1.000000000000000000, 0.9238795325112867385, 1.000000000000000000, 0.9238795325112867385, 1.000000000000000000, 0.9238795325112867385, 1.000000000000000000, 0.9238795325112867385, 1.000000000000000000, 0.9238795325112867385, 1.000000000000000000, 0.9238795325112867385, 1.000000000000000000, 0.9238795325112867385, 1.000000000000000000, 0.9238795325112867385, 1.000000000000000000, 0.9238795325112867385, 1.000000000000000000, 0.9238795325112867385, 1.000000000000000000, 0.9238795325112867385, 1.000000000000000000, 0.9238795325112867385, 1.000000000000000000, 0.9238795325112867385, 1.000000000000000000, 0.9238795325112867385, 1.000000000000000000, 0.9238795325112867385, 1.000000000000000000, 0.9238795325112867385, 1.000000000000000000, 0.9238795325112867385, 1.000000000000000000, 0.9238795325112867385, 1.000000000000000000, 0.9238795325112867385, 1.000000000000000000, 0.9238795325112867385, 1.000000000000000000, 0.9238795325112867385, 1.000000000000000000, 0.9238795325112867385, 1.000000000000000000, 0.9238795325112867385, 1.000000000000000000, 0.9238795325112867385, 1.000000000000000000, 0.9238795325112867385, 1.000000000000000000, 0.9238795325112867385, 1.000000000000000000, 0.9238795325112867385, 1.000000000000000000, 0.9238795325112867385, 1.000000000000000000, 0.9238795325112867385, 1.000000000000000000, 0.9238795325112867385, 1.000000000000000000, 0.9238795325112867385, 1.000000000000000000, 0.9238795325112867385, 1.000000000000000000, 0.9238795325112867385, 1.000000000000000000, 0.9238795325112867385, 1.000000000000000000, 0.9238795325112867385, 1.000000000000000000, 0.9238795325112867385, 1.000000000000000000, 0.9238795325112867385, 1.000000000000000000, 0.9238795325112867385, 1.000000000000000000, 0.9238795325112867385, 1.000000000000000000 ) ) 
 REPRESENTATION_ITEM ( '' )  );
#6402 = EDGE_CURVE ( 'NONE', #1668, #14298, #11720, .T. ) ;
#6403 = VECTOR ( 'NONE', #1431, 1000.000000000000000 ) ;
#6404 = CARTESIAN_POINT ( 'NONE',  ( -70.60000000218494165, 9.999999999999998224, 12.49999999999999289 ) ) ;
#6405 = CARTESIAN_POINT ( 'NONE',  ( 45.00000000000000000, -15.00000000000001954, 11.00000000000008882 ) ) ;
#6406 =( REPRESENTATION_RELATIONSHIP ('NONE','NONE', #8403, #18175 ) REPRESENTATION_RELATIONSHIP_WITH_TRANSFORMATION ( #22031 )SHAPE_REPRESENTATION_RELATIONSHIP( ) );
#6407 = AXIS2_PLACEMENT_3D ( 'NONE', #6671, #1251, #18039 ) ;
#6408 = CYLINDRICAL_SURFACE ( 'NONE', #21348, 4.000000000000000000 ) ;
#6409 = CARTESIAN_POINT ( 'NONE',  ( -1.432654583217639832, -3.458734125000000326, 18.87500000136560629 ) ) ;
#6410 = EDGE_CURVE ( 'NONE', #9029, #18952, #1019, .T. ) ;
#6411 = DIRECTION ( 'NONE',  ( 0.000000000000000000, 0.000000000000000000, -1.000000000000000000 ) ) ;
#6412 = CIRCLE ( 'NONE', #266, 11.00000000000000000 ) ;
#6413 = CARTESIAN_POINT ( 'NONE',  ( 70.10000000109246798, 10.85617417291294551, 12.93301269999999370 ) ) ;
#6414 = AXIS2_PLACEMENT_3D ( 'NONE', #7360, #8919, #16213 ) ;
#6415 = CARTESIAN_POINT ( 'NONE',  ( 72.50000000000000000, 9.999999999999998224, 14.99999999999999645 ) ) ;
#6416 = CARTESIAN_POINT ( 'NONE',  ( 52.72106816583844591, 13.02818770551464489, 16.17458954617363531 ) ) ;
#6417 = CARTESIAN_POINT ( 'NONE',  ( -2.117863837641485618E-16, 3.458734125000000770, 0.7375000013655954589 ) ) ;
#6418 = CARTESIAN_POINT ( 'NONE',  ( -3.458734124999999437, 1.432654583217640498, 12.62500000136560629 ) ) ;
#6419 = CARTESIAN_POINT ( 'NONE',  ( -68.05000000109247082, 12.06698730000000097, 14.99999999999999645 ) ) ;
#6420 = CARTESIAN_POINT ( 'NONE',  ( 72.50000000000000000, 9.999999999999998224, 17.49999999999999645 ) ) ;
#6421 = DIRECTION ( 'NONE',  ( -1.000000000000000000, -0.000000000000000000, 0.000000000000000000 ) ) ;
#6422 = ORIENTED_EDGE ( 'NONE', *, *, #13492, .F. ) ;
#6423 = DIRECTION ( 'NONE',  ( -1.000000000000000000, 0.000000000000000000, 0.000000000000000000 ) ) ;
#6424 = CARTESIAN_POINT ( 'NONE',  ( 2.828427124746190735, -2.828427124746189847, 2.800000002731188875 ) ) ;
#6425 = ORIENTED_EDGE ( 'NONE', *, *, #16537, .T. ) ;
#6426 = VERTEX_POINT ( 'NONE', #2457 ) ;
#6427 = CIRCLE ( 'NONE', #4512, 11.00000000000000000 ) ;
#6428 = CARTESIAN_POINT ( 'NONE',  ( 2.000000000000001776, 0.000000000000000000, 0.000000000000000000 ) ) ;
#6429 = CARTESIAN_POINT ( 'NONE',  ( 51.84375000000001421, 8.343145750507636293, 19.00000000000000000 ) ) ;
#6430 = VERTEX_POINT ( 'NONE', #1133 ) ;
#6431 = CARTESIAN_POINT ( 'NONE',  ( 1.287237434362044075, 3.875615274277557809, -3.430618716626812059 ) ) ;
#6432 = CIRCLE ( 'NONE', #7584, 4.000000000000001776 ) ;
#6433 = EDGE_CURVE ( 'NONE', #7689, #13210, #10656, .T. ) ;
#6434 = EDGE_CURVE ( 'NONE', #3314, #683, #19114, .T. ) ;
#6435 = CARTESIAN_POINT ( 'NONE',  ( 68.35000000109248219, 8.538419263543524096, 13.53841926354352054 ) ) ;
#6436 = CARTESIAN_POINT ( 'NONE',  ( 69.40000000109246514, 9.143825827087050939, 12.93301269999999370 ) ) ;
#6437 = ADVANCED_FACE ( 'NONE', ( #17088 ), #11838, .T. ) ;
#6438 = ORIENTED_EDGE ( 'NONE', *, *, #18002, .T. ) ;
#6439 = EDGE_CURVE ( 'NONE', #19783, #9681, #8235, .T. ) ;
#6440 = AXIS2_PLACEMENT_3D ( 'NONE', #2732, #15351, #4768 ) ;
#6441 = CARTESIAN_POINT ( 'NONE',  ( 0.000000000000000000, 5.222868219166995729, -9.680994141368717720 ) ) ;
#6442 = CARTESIAN_POINT ( 'NONE',  ( 57.37500000000000000, 7.171572875253794166, 12.17157287525381726 ) ) ;
#6443 = FACE_OUTER_BOUND ( 'NONE', #9114, .T. ) ;
#6444 = CARTESIAN_POINT ( 'NONE',  ( -3.458734124999998105, 1.432654583217640276, 18.37500000136560629 ) ) ;
#6445 = FACE_OUTER_BOUND ( 'NONE', #16678, .T. ) ;
#6446 = CIRCLE ( 'NONE', #21703, 4.000000000000000888 ) ;
#6447 = FACE_OUTER_BOUND ( 'NONE', #9497, .T. ) ;
#6448 = ORIENTED_EDGE ( 'NONE', *, *, #2055, .F. ) ;
#6449 = LINE ( 'NONE', #15688, #2298 ) ;
#6450 = COLOUR_RGB ( '', 0.08235294, 0.09019608, 0.10196078) ;
#6451 = DIRECTION ( 'NONE',  ( -0.000000000000000000, -0.000000000000000000, 1.000000000000000000 ) ) ;
#6452 = DIRECTION ( 'NONE',  ( -1.000000000000000000, -7.703719777548943412E-32, 0.000000000000000000 ) ) ;
#6453 = ORIENTED_EDGE ( 'NONE', *, *, #1272, .F. ) ;
#6454 = DIRECTION ( 'NONE',  ( -0.000000000000000000, -0.000000000000000000, -1.000000000000000000 ) ) ;
#6455 = DIRECTION ( 'NONE',  ( -1.000000000000000000, -0.000000000000000000, -0.000000000000000000 ) ) ;
#6456 = DIRECTION ( 'NONE',  ( -1.000000000000000000, 0.000000000000000000, -0.000000000000000000 ) ) ;
#6457 = EDGE_CURVE ( 'NONE', #3496, #7262, #22111, .T. ) ;
#6458 = DIRECTION ( 'NONE',  ( -1.000000000000000000, 0.000000000000000000, 1.224646799147352961E-16 ) ) ;
#6459 = ORIENTED_EDGE ( 'NONE', *, *, #2192, .T. ) ;
#6460 = CARTESIAN_POINT ( 'NONE',  ( 4.350941807883110357, 4.993536075455422996, -3.633174458636621917 ) ) ;
#6461 = ORIENTED_EDGE ( 'NONE', *, *, #16570, .F. ) ;
#6462 = CIRCLE ( 'NONE', #16039, 4.999999999999997335 ) ;
#6463 = CARTESIAN_POINT ( 'NONE',  ( 71.65000000109247935, 9.999999999999998224, 12.93301269999999192 ) ) ;
#6464 = EDGE_CURVE ( 'NONE', #433, #3718, #8350, .T. ) ;
#6465 = CARTESIAN_POINT ( 'NONE',  ( 71.10000000218494165, 8.232233047033627571, 16.76776695296636532 ) ) ;
#6466 = CARTESIAN_POINT ( 'NONE',  ( 4.000000000000001776, -1.656854249492379694, 19.43750000000001066 ) ) ;
#6467 = CIRCLE ( 'NONE', #9920, 4.714285714285714413 ) ;
#6468 = DIRECTION ( 'NONE',  ( -1.000000000000000000, 0.000000000000000000, 0.000000000000000000 ) ) ;
#6469 = CARTESIAN_POINT ( 'NONE',  ( 66.70000000109246230, 9.143825827087049163, 17.06698730000000097 ) ) ;
#6470 = ADVANCED_FACE ( 'NONE', ( #10280 ), #17333, .F. ) ;
#6471 = ORIENTED_EDGE ( 'NONE', *, *, #18420, .F. ) ;
#6472 = EDGE_CURVE ( 'NONE', #21867, #9681, #12075, .T. ) ;
#6473 = DIRECTION ( 'NONE',  ( 0.000000000000000000, 0.000000000000000000, 1.000000000000000000 ) ) ;
#6474 = CIRCLE ( 'NONE', #1475, 5.000000000000000888 ) ;
#6475 = CARTESIAN_POINT ( 'NONE',  ( 68.95000000109247651, 11.46158073645647235, 16.46158073645647235 ) ) ;
#6476 = CARTESIAN_POINT ( 'NONE',  ( 1.025207404391860050E-15, 3.458734125000000326, 13.18750000136560452 ) ) ;
#6477 = CARTESIAN_POINT ( 'NONE',  ( 71.00000000218494733, 9.999999999999998224, 17.49999999999999645 ) ) ;
#6478 = AXIS2_PLACEMENT_3D ( 'NONE', #4193, #17015, #4776 ) ;
#6479 = PLANE ( 'NONE',  #5020 ) ;
#6480 = ORIENTED_EDGE ( 'NONE', *, *, #9820, .T. ) ;
#6481 = CARTESIAN_POINT ( 'NONE',  ( -2.021686707278909978, 2.813123132921495628, -3.295601554149325541 ) ) ;
#6482 = FACE_OUTER_BOUND ( 'NONE', #17566, .T. ) ;
#6483 = CARTESIAN_POINT ( 'NONE',  ( 1.025207404391860050E-15, 3.458734125000000326, 11.18750000136560452 ) ) ;
#6484 = CARTESIAN_POINT ( 'NONE',  ( -4.000000000000000888, 1.656854249492380582, -0.7624999999999970690 ) ) ;
#6485 = CYLINDRICAL_SURFACE ( 'NONE', #23270, 6.000000000000021316 ) ;
#6486 = ORIENTED_EDGE ( 'NONE', *, *, #9854, .T. ) ;
#6487 = DIRECTION ( 'NONE',  ( 0.000000000000000000, 0.000000000000000000, 1.000000000000000000 ) ) ;
#6488 = VERTEX_POINT ( 'NONE', #8479 ) ;
#6489 = CARTESIAN_POINT ( 'NONE',  ( -67.40000000109247935, 10.85617417291294551, 17.06698729999999742 ) ) ;
#6490 = AXIS2_PLACEMENT_3D ( 'NONE', #3059, #8705, #10405 ) ;
#6491 = ORIENTED_EDGE ( 'NONE', *, *, #1593, .F. ) ;
#6492 = DIRECTION ( 'NONE',  ( 1.000000000000000000, 7.703719777548943412E-32, 0.000000000000000000 ) ) ;
#6493 = ORIENTED_EDGE ( 'NONE', *, *, #2441, .T. ) ;
#6494 = VERTEX_POINT ( 'NONE', #15783 ) ;
#6495 = CARTESIAN_POINT ( 'NONE',  ( 1.025207404391860050E-15, 3.458734125000000770, 13.43750000136560452 ) ) ;
#6496 = VECTOR ( 'NONE', #15587, 1000.000000000000000 ) ;
#6497 = DIRECTION ( 'NONE',  ( 1.000000000000000000, -0.000000000000000000, -0.000000000000000000 ) ) ;
#6498 = AXIS2_PLACEMENT_3D ( 'NONE', #20677, #2471, #22347 ) ;
#6499 = CARTESIAN_POINT ( 'NONE',  ( -66.80000000218494449, 12.50000000000000000, 14.99999999999999645 ) ) ;
#6500 = CARTESIAN_POINT ( 'NONE',  ( 66.00000000109247367, 9.143825827087052716, 12.93301269999999192 ) ) ;
#6501 = EDGE_CURVE ( 'NONE', #11365, #11624, #17130, .T. ) ;
#6502 = EDGE_CURVE ( 'NONE', #15405, #10489, #20120, .T. ) ;
#6503 = CARTESIAN_POINT ( 'NONE',  ( -70.45000000000000284, 8.964466094067258695, 12.49999999999999289 ) ) ;
#6504 = STYLED_ITEM ( 'NONE', ( #10649 ), #22288 ) ;
#6505 = CARTESIAN_POINT ( 'NONE',  ( -10.00000000000000000, 0.000000000000000000, 0.000000000000000000 ) ) ;
#6506 = CARTESIAN_POINT ( 'NONE',  ( 58.09143183416158962, 11.72490539043799984, 11.02818770551463246 ) ) ;
#6507 = DIRECTION ( 'NONE',  ( 1.224646799147353207E-16, -0.000000000000000000, 1.000000000000000000 ) ) ;
#6508 =( BOUNDED_CURVE ( )  B_SPLINE_CURVE ( 2, ( #19962, #23689, #1395, #5242, #21874, #16278, #7179, #21757, #12346 ),
 .UNSPECIFIED., .F., .F. ) 
 B_SPLINE_CURVE_WITH_KNOTS ( ( 3, 2, 2, 2, 3 ),
 ( 0.5625000000000008882, 0.5781250000000007772, 0.5937500000000006661, 0.6093750000000006661, 0.6250000000000005551 ),
 .UNSPECIFIED. ) 
 CURVE ( )  GEOMETRIC_REPRESENTATION_ITEM ( )  RATIONAL_B_SPLINE_CURVE ( ( 0.9999999999999956701, 0.9238795325112910684, 1.000000000000000000, 0.9238795325112867385, 1.000000000000000000, 0.9238795325112867385, 1.000000000000000000, 0.9238795325112840739, 1.000000000000002665 ) ) 
 REPRESENTATION_ITEM ( '' )  );
#6509 = CARTESIAN_POINT ( 'NONE',  ( 1.432654583217640276, 3.458734125000000770, 1.675000001365597235 ) ) ;
#6510 = CARTESIAN_POINT ( 'NONE',  ( 0.000000000000000000, 1.178949249685212974, -2.042000000000001148 ) ) ;
#6511 = CARTESIAN_POINT ( 'NONE',  ( 1.656854249492381470, 4.000000000000000000, 11.81250000273119838 ) ) ;
#6512 = DIRECTION ( 'NONE',  ( 0.000000000000000000, 0.000000000000000000, 1.000000000000000000 ) ) ;
#6513 = VECTOR ( 'NONE', #12026, 1000.000000000000000 ) ;
#6514 = AXIS2_PLACEMENT_3D ( 'NONE', #7220, #9143, #14412 ) ;
#6515 = VERTEX_POINT ( 'NONE', #12675 ) ;
#6516 = CARTESIAN_POINT ( 'NONE',  ( 2.500000000000000000, -2.629050547790028551E-15, -2.041999999999999815 ) ) ;
#6517 = VERTEX_POINT ( 'NONE', #8701 ) ;
#6518 = CARTESIAN_POINT ( 'NONE',  ( 60.81018183416157541, 14.00000000000000000, 15.06805114094561304 ) ) ;
#6519 = CARTESIAN_POINT ( 'NONE',  ( -3.458734125000000326, 1.432654583217640276, 0.6750000013655963471 ) ) ;
#6520 = ORIENTED_EDGE ( 'NONE', *, *, #13815, .F. ) ;
#6521 = VECTOR ( 'NONE', #11858, 1000.000000000000000 ) ;
#6522 = CARTESIAN_POINT ( 'NONE',  ( 5.000000000000000888, 0.000000000000000000, 0.000000000000000000 ) ) ;
#6523 = VECTOR ( 'NONE', #19072, 1000.000000000000000 ) ;
#6524 = ORIENTED_EDGE ( 'NONE', *, *, #18003, .T. ) ;
#6525 = CARTESIAN_POINT ( 'NONE',  ( 4.000000000000000888, 4.898587196589412829E-16, 19.50000000000001066 ) ) ;
#6526 = ORIENTED_EDGE ( 'NONE', *, *, #7766, .F. ) ;
#6527 = CARTESIAN_POINT ( 'NONE',  ( 56.09606816583844591, 11.17458954617364242, 11.97181229448534800 ) ) ;
#6528 = CARTESIAN_POINT ( 'NONE',  ( -67.95000000218495018, 7.499999999999995559, 16.03553390593273420 ) ) ;
#6529 = CARTESIAN_POINT ( 'NONE',  ( -3.458734125000000770, 0.000000000000000000, -3.012499998634404541 ) ) ;
#6530 = CARTESIAN_POINT ( 'NONE',  ( -72.00000000109245946, 12.06698730000000275, 14.14382582708705094 ) ) ;
#6531 = CARTESIAN_POINT ( 'NONE',  ( 0.000000000000000000, 0.000000000000000000, -3.674599999999999866 ) ) ;
#6532 = CARTESIAN_POINT ( 'NONE',  ( 2.828427124746191179, 2.828427124746190291, 14.75000000273119660 ) ) ;
#6533 = CARTESIAN_POINT ( 'NONE',  ( 58.87500000000000711, 7.878679656440349177, 12.87867965644035984 ) ) ;
#6534 = AXIS2_PLACEMENT_3D ( 'NONE', #18908, #7442, #351 ) ;
#6535 = CARTESIAN_POINT ( 'NONE',  ( 69.70000000109246230, 9.143825827087049163, 17.06698729999999742 ) ) ;
#6536 = CARTESIAN_POINT ( 'NONE',  ( 71.00000000218494733, 9.999999999999998224, 17.49999999999999645 ) ) ;
#6537 = STYLED_ITEM ( 'NONE', ( #214 ), #449 ) ;
#6538 = CARTESIAN_POINT ( 'NONE',  ( 57.03356816583845301, 11.31069182806492712, 17.97181229448534623 ) ) ;
#6539 = PRODUCT_DEFINITION ( 'UNKNOWN', '', #13758, #21037 ) ;
#6540 = CARTESIAN_POINT ( 'NONE',  ( -2.445694354108820523, 2.445694354108820523, -0.1374999986344035974 ) ) ;
#6541 = CARTESIAN_POINT ( 'NONE',  ( 2.445694354108822299, -2.445694354108820079, 12.06250000136560629 ) ) ;
#6542 = CARTESIAN_POINT ( 'NONE',  ( -10.00000000000000000, 0.000000000000000000, 0.000000000000000000 ) ) ;
#6543 = CARTESIAN_POINT ( 'NONE',  ( -69.85000000109246798, 9.999999999999998224, 17.06698730000000097 ) ) ;
#6544 = ADVANCED_FACE ( 'NONE', ( #10514, #19812 ), #14334, .T. ) ;
#6545 = ORIENTED_EDGE ( 'NONE', *, *, #16954, .F. ) ;
#6546 = DIRECTION ( 'NONE',  ( 0.000000000000000000, 0.000000000000000000, -1.000000000000000000 ) ) ;
#6547 = DIRECTION ( 'NONE',  ( -1.000000000000000000, 0.000000000000000000, 0.000000000000000000 ) ) ;
#6548 = ORIENTED_EDGE ( 'NONE', *, *, #6031, .T. ) ;
#6549 = CARTESIAN_POINT ( 'NONE',  ( -3.999999999999998224, -1.656854249492383024, 15.18750000273119660 ) ) ;
#6550 = CARTESIAN_POINT ( 'NONE',  ( -1.656854249492380804, 4.000000000000000000, 2.237500002731187987 ) ) ;
#6551 = EDGE_LOOP ( 'NONE', ( #2325, #14864, #15138, #12605, #11231 ) ) ;
#6552 = ORIENTED_EDGE ( 'NONE', *, *, #11023, .T. ) ;
#6553 = CARTESIAN_POINT ( 'NONE',  ( -3.250000000000004885, -5.629165124598848990, -3.700000000000000178 ) ) ;
#6554 = CARTESIAN_POINT ( 'NONE',  ( 35.00000000000000000, 4.500000000000001776, -20.00000000000000355 ) ) ;
#6555 = ORIENTED_EDGE ( 'NONE', *, *, #18730, .T. ) ;
#6556 = FACE_OUTER_BOUND ( 'NONE', #22102, .T. ) ;
#6557 = TOROIDAL_SURFACE ( 'NONE', #8103, 5.479999999999998650, 1.020000000000000018 ) ;
#6558 = CARTESIAN_POINT ( 'NONE',  ( 68.00000000109247367, 10.85617417291294551, 17.06698729999999742 ) ) ;
#6559 = CARTESIAN_POINT ( 'NONE',  ( 66.65000000109247935, 9.999999999999998224, 17.06698730000000097 ) ) ;
#6560 = ORIENTED_EDGE ( 'NONE', *, *, #16708, .F. ) ;
#6561 = MANIFOLD_SOLID_BREP ( 'M5 Clearance Hole1', #8969 ) ;
#6562 = CARTESIAN_POINT ( 'NONE',  ( 0.000000000000000000, 0.000000000000000000, 2.040000000000001812 ) ) ;
#6563 = CARTESIAN_POINT ( 'NONE',  ( 55.31250000000000711, 14.00000000000000000, 14.99999999999997691 ) ) ;
#6564 = CARTESIAN_POINT ( 'NONE',  ( -2.445694354108819635, -2.445694354108820523, 2.862500001365597235 ) ) ;
#6565 = CARTESIAN_POINT ( 'NONE',  ( 1.872352939448454495E-15, -3.458734125000000326, 17.68750000136560274 ) ) ;
#6566 = CARTESIAN_POINT ( 'NONE',  ( 5.000000000000000888, 0.000000000000000000, 4.000000000000000000 ) ) ;
#6567 = EDGE_CURVE ( 'NONE', #11236, #5065, #6432, .T. ) ;
#6568 = DIRECTION ( 'NONE',  ( 0.000000000000000000, 0.000000000000000000, 1.000000000000000000 ) ) ;
#6569 = VERTEX_POINT ( 'NONE', #23529 ) ;
#6570 = DIRECTION ( 'NONE',  ( 0.000000000000000000, -1.000000000000000000, 0.000000000000000000 ) ) ;
#6571 = EDGE_CURVE ( 'NONE', #2236, #12336, #16748, .T. ) ;
#6572 = DIRECTION ( 'NONE',  ( -0.000000000000000000, -0.000000000000000000, 1.000000000000000000 ) ) ;
#6573 = DIRECTION ( 'NONE',  ( 0.000000000000000000, 0.000000000000000000, -1.000000000000000000 ) ) ;
#6574 = VERTEX_POINT ( 'NONE', #12310 ) ;
#6575 = CARTESIAN_POINT ( 'NONE',  ( -60.00000000000000711, 15.00000000000000000, 25.00000000000001421 ) ) ;
#6576 = CARTESIAN_POINT ( 'NONE',  ( 2.435583919667260400, -11.25000000000000355, 5.000000000000079936 ) ) ;
#6577 = ADVANCED_FACE ( 'NONE', ( #14222 ), #6667, .F. ) ;
#6578 = FACE_OUTER_BOUND ( 'NONE', #21947, .T. ) ;
#6579 = ORIENTED_EDGE ( 'NONE', *, *, #13246, .F. ) ;
#6580 = CARTESIAN_POINT ( 'NONE',  ( -1.520000000000000462, 0.000000000000000000, 0.000000000000000000 ) ) ;
#6581 = ORIENTED_EDGE ( 'NONE', *, *, #15741, .F. ) ;
#6582 = CARTESIAN_POINT ( 'NONE',  ( 71.80000000109247082, 12.06698729999999919, 14.14382582708705094 ) ) ;
#6583 = CARTESIAN_POINT ( 'NONE',  ( 71.80000000218494449, 9.999999999999998224, 17.49999999999999645 ) ) ;
#6584 = CARTESIAN_POINT ( 'NONE',  ( -2.247776618166720475, 3.308700692843488333, 10.40809237798934994 ) ) ;
#6585 = CARTESIAN_POINT ( 'NONE',  ( 4.999999999999999112, -9.314797388894900720, 1.239665997526853580 ) ) ;
#6586 = CARTESIAN_POINT ( 'NONE',  ( 68.20000000109246230, 10.85617417291294551, 17.06698730000000097 ) ) ;
#6587 = ORIENTED_EDGE ( 'NONE', *, *, #8046, .T. ) ;
#6588 = CARTESIAN_POINT ( 'NONE',  ( 1.799999999999999156, 0.000000000000000000, 0.000000000000000000 ) ) ;
#6589 = EDGE_CURVE ( 'NONE', #2537, #18556, #9500, .T. ) ;
#6590 = CARTESIAN_POINT ( 'NONE',  ( 19.99999999999999645, 16.40063509461079860, -43.12916512459904084 ) ) ;
#6591 = CARTESIAN_POINT ( 'NONE',  ( 69.90000000109246514, 9.143825827087049163, 17.06698729999999742 ) ) ;
#6592 = CARTESIAN_POINT ( 'NONE',  ( 2.445694354108822299, -2.445694354108820079, 17.06250000136560629 ) ) ;
#6593 = DIRECTION ( 'NONE',  ( 1.000000000000000000, 0.000000000000000000, 0.000000000000000000 ) ) ;
#6594 = CARTESIAN_POINT ( 'NONE',  ( 44.71007725323381976, -9.000000000000003553, 10.29587622221672127 ) ) ;
#6595 = ORIENTED_EDGE ( 'NONE', *, *, #13517, .T. ) ;
#6596 = CARTESIAN_POINT ( 'NONE',  ( -4.000000000000000000, 0.000000000000000000, -1.699999999999998401 ) ) ;
#6597 = EDGE_CURVE ( 'NONE', #11306, #19691, #23290, .T. ) ;
#6598 = DIRECTION ( 'NONE',  ( -0.000000000000000000, -0.000000000000000000, 1.000000000000000000 ) ) ;
#6599 = CARTESIAN_POINT ( 'NONE',  ( 0.000000000000000000, 10.82112760146736363, 1.975651141462276161 ) ) ;
#6600 = CARTESIAN_POINT ( 'NONE',  ( 9.399474963057187438, 1.700533789607089563, 10.00000000000008882 ) ) ;
#6601 = VERTEX_POINT ( 'NONE', #1722 ) ;
#6602 = CARTESIAN_POINT ( 'NONE',  ( 2.828427124746192067, -2.828427124746189847, 13.50000000273119660 ) ) ;
#6603 = EDGE_LOOP ( 'NONE', ( #20716, #21468, #4243, #22139 ) ) ;
#6604 = CARTESIAN_POINT ( 'NONE',  ( -66.15000000109247935, 8.538419263543524096, 13.53841926354352054 ) ) ;
#6605 = ITEM_DEFINED_TRANSFORMATION ( 'NONE', 'NONE', #19104,  #7318 ) ;
#6606 = EDGE_CURVE ( 'NONE', #3610, #4306, #1490, .T. ) ;
#6607 = ORIENTED_EDGE ( 'NONE', *, *, #2874, .F. ) ;
#6608 = CARTESIAN_POINT ( 'NONE',  ( -66.15000000218496723, 11.03553390593268624, 17.50000000000005329 ) ) ;
#6609 = ORIENTED_EDGE ( 'NONE', *, *, #18290, .T. ) ;
#6610 = ADVANCED_FACE ( 'NONE', ( #4853, #19461 ), #3056, .T. ) ;
#6611 = ORIENTED_EDGE ( 'NONE', *, *, #12027, .F. ) ;
#6612 = CARTESIAN_POINT ( 'NONE',  ( -2.445694354108819191, 2.445694354108820523, 11.56250000136560629 ) ) ;
#6613 = CARTESIAN_POINT ( 'NONE',  ( 51.46875000000000000, 6.999999999999992895, 13.75735931288071967 ) ) ;
#6614 = CARTESIAN_POINT ( 'NONE',  ( 9.546947090716562556, -8.974600000000002353, 5.000000000000079936 ) ) ;
#6615 = FACE_OUTER_BOUND ( 'NONE', #188, .T. ) ;
#6616 = CARTESIAN_POINT ( 'NONE',  ( -69.64999999999999147, 8.964466094067258695, 12.49999999999999289 ) ) ;
#6617 = CARTESIAN_POINT ( 'NONE',  ( 5.000000000000000888, 0.000000000000000000, 0.000000000000000000 ) ) ;
#6618 = CARTESIAN_POINT ( 'NONE',  ( 53.12268183416157541, 12.07320092032950676, 17.16943976678977180 ) ) ;
#6619 = CARTESIAN_POINT ( 'NONE',  ( 60.00000000000004974, 13.00472853162060538, 15.58205920398491173 ) ) ;
#6620 = CARTESIAN_POINT ( 'NONE',  ( -2.445694354108820523, 2.445694354108820523, -0.1374999986344035974 ) ) ;
#6621 = DIRECTION ( 'NONE',  ( -0.000000000000000000, -0.000000000000000000, 1.000000000000000000 ) ) ;
#6622 = DIRECTION ( 'NONE',  ( -1.000000000000000000, -0.000000000000000000, -0.000000000000000000 ) ) ;
#6623 = CARTESIAN_POINT ( 'NONE',  ( -2.828427124746189403, 2.828427124746190291, 11.00000000273119660 ) ) ;
#6624 = LINE ( 'NONE', #4586, #7678 ) ;
#6625 = ORIENTED_EDGE ( 'NONE', *, *, #9262, .T. ) ;
#6626 = CARTESIAN_POINT ( 'NONE',  ( -11.01965741966725076, -11.25000000000000355, 5.000000000000079936 ) ) ;
#6627 = ORIENTED_EDGE ( 'NONE', *, *, #17184, .F. ) ;
#6628 = CARTESIAN_POINT ( 'NONE',  ( 52.09143183416158251, 11.31069182806491291, 12.02818770551463778 ) ) ;
#6629 = CARTESIAN_POINT ( 'NONE',  ( -69.25000000109247367, 9.999999999999998224, 12.93301269999999192 ) ) ;
#6630 =( LENGTH_UNIT ( ) NAMED_UNIT ( * ) SI_UNIT ( .MILLI., .METRE. ) );
#6631 = EDGE_CURVE ( 'NONE', #20551, #15816, #22373, .T. ) ;
#6632 = ADVANCED_FACE ( 'NONE', ( #16474 ), #11215, .T. ) ;
#6633 = CARTESIAN_POINT ( 'NONE',  ( 6.353591512924457348E-16, -3.458734125000000326, 1.987500001365596569 ) ) ;
#6634 = ORIENTED_EDGE ( 'NONE', *, *, #8560, .T. ) ;
#6635 = DIRECTION ( 'NONE',  ( 0.3420201433256622181, 0.9396926207859107594, -6.162975822039141593E-32 ) ) ;
#6636 = EDGE_CURVE ( 'NONE', #4939, #2701, #20278, .T. ) ;
#6637 = VECTOR ( 'NONE', #6546, 1000.000000000000000 ) ;
#6638 = VECTOR ( 'NONE', #1187, 1000.000000000000000 ) ;
#6639 = ORIENTED_EDGE ( 'NONE', *, *, #17117, .T. ) ;
#6640 = CARTESIAN_POINT ( 'NONE',  ( -90.00000000000000000, 0.000000000000000000, 0.000000000000000000 ) ) ;
#6641 = VERTEX_POINT ( 'NONE', #23651 ) ;
#6642 = CARTESIAN_POINT ( 'NONE',  ( 57.97106816583845301, 6.971812294485350670, 13.82541045382635403 ) ) ;
#6643 = CARTESIAN_POINT ( 'NONE',  ( -66.45000000218495018, 7.499999999999995559, 13.96446609406725692 ) ) ;
#6644 = FACE_OUTER_BOUND ( 'NONE', #12367, .T. ) ;
#6645 = CARTESIAN_POINT ( 'NONE',  ( -71.90000000109246514, 10.85617417291294551, 12.93301269999999370 ) ) ;
#6646 =( BOUNDED_CURVE ( )  B_SPLINE_CURVE ( 2, ( #3697, #4061, #22010, #2014, #5624, #5506, #22131, #2381, #9711 ),
 .UNSPECIFIED., .F., .F. ) 
 B_SPLINE_CURVE_WITH_KNOTS ( ( 3, 2, 2, 2, 3 ),
 ( 0.000000000000000000, 0.01250000000000000243, 0.02500000000000000486, 0.03749999999999999861, 0.05000000000000000971 ),
 .UNSPECIFIED. ) 
 CURVE ( )  GEOMETRIC_REPRESENTATION_ITEM ( )  RATIONAL_B_SPLINE_CURVE ( ( 1.000000000000000000, 0.9238795325112867385, 1.000000000000000000, 0.9238795325112867385, 1.000000000000000000, 0.9238795325112867385, 1.000000000000000000, 0.9238795325112867385, 1.000000000000000000 ) ) 
 REPRESENTATION_ITEM ( '' )  );
#6647 = CARTESIAN_POINT ( 'NONE',  ( 1.432654583217643163, -3.458734124999999882, 19.00000000136560629 ) ) ;
#6648 = CARTESIAN_POINT ( 'NONE',  ( 2.828427124746192067, -2.828427124746189847, 14.50000000273119660 ) ) ;
#6649 = CYLINDRICAL_SURFACE ( 'NONE', #13532, 8.749000000000002331 ) ;
#6650 = CARTESIAN_POINT ( 'NONE',  ( 68.35000000109248219, 8.538419263543524096, 13.53841926354352054 ) ) ;
#6651 = DIRECTION ( 'NONE',  ( -1.000000000000000000, 0.000000000000000000, -0.000000000000000000 ) ) ;
#6652 = CARTESIAN_POINT ( 'NONE',  ( 59.71875000000000711, 13.00000000000000711, 16.24264068711927322 ) ) ;
#6653 = AXIS2_PLACEMENT_3D ( 'NONE', #10332, #6824, #23214 ) ;
#6654 = CARTESIAN_POINT ( 'NONE',  ( -3.458734125000000326, -1.432654583217642497, 2.050000001365597679 ) ) ;
#6655 = DIRECTION ( 'NONE',  ( 0.000000000000000000, 0.3090169943749481174, -0.9510565162951533091 ) ) ;
#6656 = CARTESIAN_POINT ( 'NONE',  ( 67.49999999999998579, 12.50000000000000000, 14.99999999999999645 ) ) ;
#6657 = CARTESIAN_POINT ( 'NONE',  ( -69.20000000109246230, 7.933012699999995476, 15.85617417291294196 ) ) ;
#6658 = ORIENTED_EDGE ( 'NONE', *, *, #18404, .F. ) ;
#6659 = DIRECTION ( 'NONE',  ( -1.000000000000000000, 0.000000000000000000, 0.000000000000000000 ) ) ;
#6660 = DIRECTION ( 'NONE',  ( -1.000000000000000000, 0.000000000000000000, 0.000000000000000000 ) ) ;
#6661 = EDGE_LOOP ( 'NONE', ( #9206, #4382, #9755, #20215 ) ) ;
#6662 =( NAMED_UNIT ( * ) SI_UNIT ( $, .STERADIAN. ) SOLID_ANGLE_UNIT ( ) );
#6663 = EDGE_CURVE ( 'NONE', #8665, #1712, #22061, .T. ) ;
#6664 = CARTESIAN_POINT ( 'NONE',  ( -1.656854249492380804, 4.000000000000000000, 1.237500002731187099 ) ) ;
#6665 = VERTEX_POINT ( 'NONE', #165 ) ;
#6666 = VERTEX_POINT ( 'NONE', #9188 ) ;
#6667 = PLANE ( 'NONE',  #287 ) ;
#6668 = LINE ( 'NONE', #4856, #3738 ) ;
#6669 = ORIENTED_EDGE ( 'NONE', *, *, #11696, .F. ) ;
#6670 = CYLINDRICAL_SURFACE ( 'NONE', #23291, 2.649999999999992806 ) ;
#6671 = CARTESIAN_POINT ( 'NONE',  ( -5.564649990716551642, -8.974600000000002353, 5.000000000000079936 ) ) ;
#6672 = CARTESIAN_POINT ( 'NONE',  ( 68.75000000109245946, 11.46158073645647235, 13.53841926354352232 ) ) ;
#6673 = B_SPLINE_CURVE_WITH_KNOTS ( 'NONE', 3,
 ( #3596, #10936, #18215, #21908, #5516, #20232 ),
 .UNSPECIFIED., .F., .F.,
 ( 4, 2, 4 ),
 ( 0.000000000000000000, 0.0002095117440854740156, 0.0004190234881709480313 ),
 .UNSPECIFIED. ) ;
#6674 = FACE_OUTER_BOUND ( 'NONE', #1274, .T. ) ;
#6675 = FACE_OUTER_BOUND ( 'NONE', #12399, .T. ) ;
#6676 = CARTESIAN_POINT ( 'NONE',  ( 52.68750000000000711, 9.999999999999978684, 10.99999999999999645 ) ) ;
#6677 = FACE_OUTER_BOUND ( 'NONE', #13709, .T. ) ;
#6678 = CARTESIAN_POINT ( 'NONE',  ( -2.445694354108818303, -2.445694354108820523, 15.56250000136560629 ) ) ;
#6679 = CYLINDRICAL_SURFACE ( 'NONE', #13613, 4.000000000000000000 ) ;
#6680 = CARTESIAN_POINT ( 'NONE',  ( -66.60000000218495586, 9.999999999999998224, 12.49999999999999289 ) ) ;
#6681 = VERTEX_POINT ( 'NONE', #18378 ) ;
#6682 = CARTESIAN_POINT ( 'NONE',  ( -3.561348994077910834, 0.3690845827472539198, 2.039999999999996927 ) ) ;
#6683 = LINE ( 'NONE', #21502, #17454 ) ;
#6684 = ORIENTED_EDGE ( 'NONE', *, *, #20323, .T. ) ;
#6685 = CARTESIAN_POINT ( 'NONE',  ( -67.49999999999998579, 12.50000000000000000, 14.99999999999999645 ) ) ;
#6686 = CARTESIAN_POINT ( 'NONE',  ( 3.678949249685231848, 0.000000000000000000, 0.000000000000000000 ) ) ;
#6687 = ORIENTED_EDGE ( 'NONE', *, *, #845, .F. ) ;
#6688 = CARTESIAN_POINT ( 'NONE',  ( 60.00000000000000000, -10.00000000000000178, 17.49999999999999645 ) ) ;
#6689 = EDGE_LOOP ( 'NONE', ( #492, #21529, #7532, #21356 ) ) ;
#6690 = AXIS2_PLACEMENT_3D ( 'NONE', #21972, #3779, #11119 ) ;
#6691 = CARTESIAN_POINT ( 'NONE',  ( 54.28125000000000000, 8.343145750507600766, 11.00000000000000533 ) ) ;
#6692 = VECTOR ( 'NONE', #8117, 1000.000000000000000 ) ;
#6693 = CIRCLE ( 'NONE', #16641, 5.000000000000004441 ) ;
#6694 = LINE ( 'NONE', #19022, #16479 ) ;
#6695 = EDGE_CURVE ( 'NONE', #23104, #11298, #12333, .T. ) ;
#6696 = CARTESIAN_POINT ( 'NONE',  ( 4.000000000000001776, -1.656854249492379694, 16.43750000000001066 ) ) ;
#6697 = CARTESIAN_POINT ( 'NONE',  ( 2.499999999999999556, -9.915734732513184824, -4.762163868918378284 ) ) ;
#6698 = CARTESIAN_POINT ( 'NONE',  ( 66.65000000109247935, 9.999999999999998224, 17.06698730000000097 ) ) ;
#6699 = ORIENTED_EDGE ( 'NONE', *, *, #11564, .F. ) ;
#6700 = CARTESIAN_POINT ( 'NONE',  ( -68.95000000218495018, 8.964466094067285340, 12.49999999999996980 ) ) ;
#6701 = CARTESIAN_POINT ( 'NONE',  ( 1.656854249492383024, -3.999999999999999112, -1.262499997268811125 ) ) ;
#6702 = EDGE_CURVE ( 'NONE', #23515, #6003, #21317, .T. ) ;
#6703 = CARTESIAN_POINT ( 'NONE',  ( 67.65000000109247935, 7.933012699999995476, 14.99999999999999645 ) ) ;
#6704 = CARTESIAN_POINT ( 'NONE',  ( -3.458734124999999437, 0.000000000000000000, 19.68750000136560629 ) ) ;
#6705 = DIRECTION ( 'NONE',  ( 0.000000000000000000, 0.000000000000000000, 1.000000000000000000 ) ) ;
#6706 = CARTESIAN_POINT ( 'NONE',  ( 2.499999999999999556, 1.975651141462237970, 10.82112760146736896 ) ) ;
#6707 = SHAPE_REPRESENTATION ( 'socket head cap screw_iso_ISO 4762 M5 x 16 - 16N', ( #7318 ), #5664 ) ;
#6708 = ORIENTED_EDGE ( 'NONE', *, *, #4361, .T. ) ;
#6709 = DIRECTION ( 'NONE',  ( -1.000000000000000000, -0.000000000000000000, -0.000000000000000000 ) ) ;
#6710 = CARTESIAN_POINT ( 'NONE',  ( -19.99999999999999645, -9.000000000000003553, 10.00000000000008882 ) ) ;
#6711 = CIRCLE ( 'NONE', #7091, 0.1999999999999996503 ) ;
#6712 = CARTESIAN_POINT ( 'NONE',  ( 7.347880794884118750E-16, -4.000000000000000000, 0.6750000027311870987 ) ) ;
#6713 = DIRECTION ( 'NONE',  ( 0.000000000000000000, 0.000000000000000000, 1.000000000000000000 ) ) ;
#6714 = VERTEX_POINT ( 'NONE', #9534 ) ;
#6715 = DIRECTION ( 'NONE',  ( 0.9396926207859107594, -0.3420201433256623291, 3.697785493223492838E-32 ) ) ;
#6716 = ORIENTED_EDGE ( 'NONE', *, *, #11282, .F. ) ;
#6717 = CARTESIAN_POINT ( 'NONE',  ( 72.50000000000000000, 9.999999999999998224, 17.49999999999999645 ) ) ;
#6718 = ORIENTED_EDGE ( 'NONE', *, *, #1202, .F. ) ;
#6719 = CARTESIAN_POINT ( 'NONE',  ( -4.898587196589412829E-16, 0.000000000000000000, -4.000000000000000000 ) ) ;
#6720 = ORIENTED_EDGE ( 'NONE', *, *, #5761, .T. ) ;
#6721 =( REPRESENTATION_RELATIONSHIP ('NONE','NONE', #8403, #9307 ) REPRESENTATION_RELATIONSHIP_WITH_TRANSFORMATION ( #13334 )SHAPE_REPRESENTATION_RELATIONSHIP( ) );
#6722 = ORIENTED_EDGE ( 'NONE', *, *, #23292, .T. ) ;
#6723 = CARTESIAN_POINT ( 'NONE',  ( 3.458734125000002546, -1.432654583217639610, 11.12500000136560452 ) ) ;
#6724 = CARTESIAN_POINT ( 'NONE',  ( 52.31250000000000711, 13.00000000000000000, 14.99999999999998757 ) ) ;
#6725 = EDGE_CURVE ( 'NONE', #21534, #10010, #279, .T. ) ;
#6726 = AXIS2_PLACEMENT_3D ( 'NONE', #10482, #1332, #9629 ) ;
#6727 = CARTESIAN_POINT ( 'NONE',  ( -66.95000000218496439, 11.03553390593272887, 17.50000000000001066 ) ) ;
#6728 = EDGE_CURVE ( 'NONE', #17331, #10854, #14481, .T. ) ;
#6729 = AXIS2_PLACEMENT_3D ( 'NONE', #19707, #1745, #18160 ) ;
#6730 = CARTESIAN_POINT ( 'NONE',  ( 1.236993788156008760E-15, 0.000000000000000000, 21.31370849898476649 ) ) ;
#6731 = CARTESIAN_POINT ( 'NONE',  ( -68.95000000000000284, 11.03553390593273598, 12.49999999999999289 ) ) ;
#6732 = DIRECTION ( 'NONE',  ( 1.000000000000000000, 7.703719777548943412E-32, 0.000000000000000000 ) ) ;
#6733 = EDGE_CURVE ( 'NONE', #13557, #13221, #1959, .T. ) ;
#6734 = CARTESIAN_POINT ( 'NONE',  ( 60.00000000000001421, 13.67480539368983017, 13.43375491155203960 ) ) ;
#6735 = EDGE_CURVE ( 'NONE', #16674, #2643, #1056, .T. ) ;
#6736 = AXIS2_PLACEMENT_3D ( 'NONE', #17591, #10303, #8496 ) ;
#6737 = CARTESIAN_POINT ( 'NONE',  ( 3.458734125000000770, 4.235727675282972223E-16, 0.4875000013655969577 ) ) ;
#6738 = CARTESIAN_POINT ( 'NONE',  ( -67.55000000218494449, 12.50000000000000000, 13.96446609406725692 ) ) ;
#6739 = LINE ( 'NONE', #14046, #21114 ) ;
#6740 = CARTESIAN_POINT ( 'NONE',  ( 2.445694354108821855, -2.445694354108820079, 18.81250000136560629 ) ) ;
#6741 = CARTESIAN_POINT ( 'NONE',  ( 46.41788101966725577, -11.25000000000000355, 5.000000000000079936 ) ) ;
#6742 = VERTEX_POINT ( 'NONE', #12782 ) ;
#6743 = CARTESIAN_POINT ( 'NONE',  ( -72.05000000109247082, 9.999999999999998224, 17.06698730000000097 ) ) ;
#6744 = ORIENTED_EDGE ( 'NONE', *, *, #20068, .F. ) ;
#6745 = CARTESIAN_POINT ( 'NONE',  ( 53.31018183416157541, 12.99999999999999822, 15.06805114094562192 ) ) ;
#6746 = CARTESIAN_POINT ( 'NONE',  ( -69.10000000109248219, 7.933012699999995476, 14.14382582708705094 ) ) ;
#6747 = SHAPE_REPRESENTATION_RELATIONSHIP ( 'NONE' , 'NONE' ,  #6707, #1883 ) ;
#6748 = DIRECTION ( 'NONE',  ( -1.000000000000000000, -0.000000000000000000, -0.000000000000000000 ) ) ;
#6749 = ORIENTED_EDGE ( 'NONE', *, *, #13786, .F. ) ;
#6750 = LINE ( 'NONE', #8673, #15258 ) ;
#6751 = ORIENTED_EDGE ( 'NONE', *, *, #13943, .F. ) ;
#6752 = CARTESIAN_POINT ( 'NONE',  ( 72.50000000000000000, 9.999999999999998224, 14.99999999999999645 ) ) ;
#6753 = VERTEX_POINT ( 'NONE', #18734 ) ;
#6754 = CARTESIAN_POINT ( 'NONE',  ( 50.56481816583844591, 5.999999999999996447, 15.06805114094564502 ) ) ;
#6755 = CARTESIAN_POINT ( 'NONE',  ( -67.70000000218493597, 11.76776695296636888, 16.76776695296636532 ) ) ;
#6756 = ADVANCED_FACE ( 'NONE', ( #2323 ), #16586, .T. ) ;
#6757 = CYLINDRICAL_SURFACE ( 'NONE', #20153, 2.100000000000000089 ) ;
#6758 = DIRECTION ( 'NONE',  ( 0.3420201433256622736, -0.9396926207859106484, -1.232595164407828100E-31 ) ) ;
#6759 = CARTESIAN_POINT ( 'NONE',  ( 3.458734125000001658, 1.432654583217640498, 15.25000000136560807 ) ) ;
#6760 = CARTESIAN_POINT ( 'NONE',  ( -3.999999999999999112, 1.656854249492380804, 11.06250000273119660 ) ) ;
#6761 = CARTESIAN_POINT ( 'NONE',  ( 58.21875000000000711, 13.00000000000000711, 16.24264068711927322 ) ) ;
#6762 = CARTESIAN_POINT ( 'NONE',  ( -2.100000000000000089, 2.571758278209441957E-16, -0.2800830152838844622 ) ) ;
#6763 = EDGE_CURVE ( 'NONE', #6641, #11902, #11339, .T. ) ;
#6764 = CARTESIAN_POINT ( 'NONE',  ( 50.65856816583843880, 7.028187705514647554, 16.31069182806492179 ) ) ;
#6765 = CARTESIAN_POINT ( 'NONE',  ( -2.445694354108819635, -2.445694354108820967, 2.112500001365596791 ) ) ;
#6766 = CARTESIAN_POINT ( 'NONE',  ( 4.000000000000000888, 1.656854249492381248, 18.68750000273119483 ) ) ;
#6767 = CARTESIAN_POINT ( 'NONE',  ( -60.00000000000000711, -10.00000000000000178, 12.49999999999999467 ) ) ;
#6768 = ORIENTED_EDGE ( 'NONE', *, *, #10982, .F. ) ;
#6769 = CARTESIAN_POINT ( 'NONE',  ( 55.00000000000000711, -15.00000000000000000, 19.99999999999999645 ) ) ;
#6770 = DIRECTION ( 'NONE',  ( 0.000000000000000000, 0.000000000000000000, 1.000000000000000000 ) ) ;
#6771 = VERTEX_POINT ( 'NONE', #2196 ) ;
#6772 = CARTESIAN_POINT ( 'NONE',  ( 58.21875000000000711, 13.00000000000000711, 16.24264068711927322 ) ) ;
#6773 =( NAMED_UNIT ( * ) PLANE_ANGLE_UNIT ( ) SI_UNIT ( $, .RADIAN. ) );
#6774 = CARTESIAN_POINT ( 'NONE',  ( -1.656854249492381248, -3.999999999999999112, -1.387499997268811125 ) ) ;
#6775 = ORIENTED_EDGE ( 'NONE', *, *, #22976, .T. ) ;
#6776 = EDGE_LOOP ( 'NONE', ( #6779, #15584, #2409, #22500 ) ) ;
#6777 = CARTESIAN_POINT ( 'NONE',  ( 0.000000000000000000, 0.000000000000000000, 0.000000000000000000 ) ) ;
#6778 = FACE_OUTER_BOUND ( 'NONE', #19870, .T. ) ;
#6779 = ORIENTED_EDGE ( 'NONE', *, *, #5825, .F. ) ;
#6780 = CARTESIAN_POINT ( 'NONE',  ( 4.000000000000000000, -2.309401076758514915, -3.433295621305383349 ) ) ;
#6781 = CARTESIAN_POINT ( 'NONE',  ( 50.00000000000000000, 14.69846310392956745, 35.82846581308617573 ) ) ;
#6782 = EDGE_LOOP ( 'NONE', ( #23335, #12894 ) ) ;
#6783 = CARTESIAN_POINT ( 'NONE',  ( 66.40000000109247935, 10.85617417291294551, 17.06698729999999742 ) ) ;
#6784 = TOROIDAL_SURFACE ( 'NONE', #700, 8.239200000000002078, 0.03079999999999879709 ) ;
#6785 = CARTESIAN_POINT ( 'NONE',  ( 71.84999999999999432, 7.499999999999995559, 16.03553390593273420 ) ) ;
#6786 = ADVANCED_FACE ( 'NONE', ( #16831 ), #7597, .T. ) ;
#6787 = CARTESIAN_POINT ( 'NONE',  ( -65.65000000218495302, 7.499999999999996447, 13.96446609406725514 ) ) ;
#6788 = B_SPLINE_CURVE_WITH_KNOTS ( 'NONE', 3,
 ( #12345, #15704, #8387, #933, #4772, #12108 ),
 .UNSPECIFIED., .F., .F.,
 ( 4, 2, 4 ),
 ( 2.380733003139562494E-07, 0.001898835937927376150, 0.003797433802554438069 ),
 .UNSPECIFIED. ) ;
#6789 = LINE ( 'NONE', #14110, #13794 ) ;
#6790 = CARTESIAN_POINT ( 'NONE',  ( 55.43981816583843170, 10.06805114094564857, 19.00000000000000000 ) ) ;
#6791 = CARTESIAN_POINT ( 'NONE',  ( 2.445694354108820079, 2.445694354108820523, 2.362500001365596791 ) ) ;
#6792 = CARTESIAN_POINT ( 'NONE',  ( 2.445694354108821855, -2.445694354108820079, 15.81250000136560629 ) ) ;
#6793 = LINE ( 'NONE', #21025, #4012 ) ;
#6794 = CONICAL_SURFACE ( 'NONE', #23223, 6.500000000000000888, 1.047197551196596521 ) ;
#6795 = LINE ( 'NONE', #14473, #22001 ) ;
#6796 = ORIENTED_EDGE ( 'NONE', *, *, #9994, .T. ) ;
#6797 = CARTESIAN_POINT ( 'NONE',  ( -2.154698047631601110, 3.153627145295581524, 2.039999999999997371 ) ) ;
#6798 = CARTESIAN_POINT ( 'NONE',  ( -2.000000000000000888, 6.543750000000021494, 0.000000000000000000 ) ) ;
#6799 = DIRECTION ( 'NONE',  ( 0.000000000000000000, 0.000000000000000000, 1.000000000000000000 ) ) ;
#6800 = COLOUR_RGB ( '', 0.66274510, 0.83137255, 0.94901961) ;
#6801 = AXIS2_PLACEMENT_3D ( 'NONE', #10783, #17598, #21507 ) ;
#6802 = ORIENTED_EDGE ( 'NONE', *, *, #12223, .F. ) ;
#6803 = FACE_BOUND ( 'NONE', #3252, .T. ) ;
#6804 = CARTESIAN_POINT ( 'NONE',  ( 72.05000000109247082, 9.999999999999998224, 17.06698730000000097 ) ) ;
#6805 = CARTESIAN_POINT ( 'NONE',  ( 59.71875000000000711, 14.00000000000001066, 16.65685424949235482 ) ) ;
#6806 = ORIENTED_EDGE ( 'NONE', *, *, #16256, .T. ) ;
#6807 = CARTESIAN_POINT ( 'NONE',  ( -69.34999999999999432, 8.964466094067214286, 17.49999999999996092 ) ) ;
#6808 = VERTEX_POINT ( 'NONE', #13251 ) ;
#6809 = CARTESIAN_POINT ( 'NONE',  ( 53.43750000000000711, 10.00000000000001776, 18.99999999999999645 ) ) ;
#6810 = CARTESIAN_POINT ( 'NONE',  ( 68.20000000218495018, 9.999999999999998224, 12.49999999999999289 ) ) ;
#6811 = AXIS2_PLACEMENT_3D ( 'NONE', #12230, #6468, #8272 ) ;
#6812 = DIRECTION ( 'NONE',  ( 0.000000000000000000, 0.000000000000000000, 1.000000000000000000 ) ) ;
#6813 = DIRECTION ( 'NONE',  ( -1.000000000000000000, 0.000000000000000000, 0.000000000000000000 ) ) ;
#6814 = CARTESIAN_POINT ( 'NONE',  ( 67.75000000109245946, 8.538419263543524096, 13.53841926354352054 ) ) ;
#6815 = VERTEX_POINT ( 'NONE', #14582 ) ;
#6816 = DIRECTION ( 'NONE',  ( -1.224646799147353207E-16, 0.000000000000000000, -1.000000000000000000 ) ) ;
#6817 = CARTESIAN_POINT ( 'NONE',  ( 72.50000000000000000, 9.999999999999998224, 17.49999999999999645 ) ) ;
#6818 = CYLINDRICAL_SURFACE ( 'NONE', #8788, 4.000000000000000888 ) ;
#6819 = CARTESIAN_POINT ( 'NONE',  ( 3.458734125000002546, -1.432654583217639610, 19.12500000136560629 ) ) ;
#6820 = CARTESIAN_POINT ( 'NONE',  ( 21.00000000000000355, 0.000000000000000000, 0.000000000000000000 ) ) ;
#6821 = CARTESIAN_POINT ( 'NONE',  ( -6.499999999999999112, -1.264206540070614615, -3.645490429492275197 ) ) ;
#6822 = VERTEX_POINT ( 'NONE', #4598 ) ;
#6823 = CARTESIAN_POINT ( 'NONE',  ( -3.149734950108402654, 1.481481450868026295, -3.295601554149321988 ) ) ;
#6824 = DIRECTION ( 'NONE',  ( 1.000000000000000000, -0.000000000000000000, -0.000000000000000000 ) ) ;
#6825 = FILL_AREA_STYLE ('',( #23215 ) ) ;
#6826 = EDGE_LOOP ( 'NONE', ( #570, #14219, #20776, #20249 ) ) ;
#6827 = VECTOR ( 'NONE', #14874, 1000.000000000000114 ) ;
#6828 = EDGE_CURVE ( 'NONE', #13267, #3743, #16946, .T. ) ;
#6829 = FACE_OUTER_BOUND ( 'NONE', #8610, .T. ) ;
#6830 = CARTESIAN_POINT ( 'NONE',  ( 3.458734125000000326, 4.235727675282971730E-16, -0.7624999986344040970 ) ) ;
#6831 = CARTESIAN_POINT ( 'NONE',  ( 45.00000000000000000, 2.399706452296377801, 55.00000000000021316 ) ) ;
#6832 = EDGE_LOOP ( 'NONE', ( #8883, #19025, #13151 ) ) ;
#6833 = DIRECTION ( 'NONE',  ( 0.000000000000000000, 0.000000000000000000, 1.000000000000000000 ) ) ;
#6834 = ORIENTED_EDGE ( 'NONE', *, *, #15797, .T. ) ;
#6835 = CARTESIAN_POINT ( 'NONE',  ( -3.999999999999999112, 1.656854249492380582, 13.06250000273119660 ) ) ;
#6836 = VECTOR ( 'NONE', #9125, 1000.000000000000000 ) ;
#6837 = ORIENTED_EDGE ( 'NONE', *, *, #12604, .T. ) ;
#6838 = CARTESIAN_POINT ( 'NONE',  ( 3.458734125000001658, 4.235727675282972223E-16, 14.18750000136560629 ) ) ;
#6839 = ADVANCED_FACE ( 'NONE', ( #2677 ), #7968, .T. ) ;
#6840 = CARTESIAN_POINT ( 'NONE',  ( -66.24999999999998579, 7.499999999999996447, 16.03553390593273775 ) ) ;
#6841 = FACE_OUTER_BOUND ( 'NONE', #15409, .T. ) ;
#6842 = CARTESIAN_POINT ( 'NONE',  ( -67.70000000000000284, 9.999999999999998224, 17.49999999999999645 ) ) ;
#6843 = DIRECTION ( 'NONE',  ( 1.000000000000000000, 0.000000000000000000, 0.000000000000000000 ) ) ;
#6844 = VECTOR ( 'NONE', #19554, 1000.000000000000000 ) ;
#6845 = CARTESIAN_POINT ( 'NONE',  ( -71.79999999999998295, 8.232233047033627571, 16.76776695296636532 ) ) ;
#6846 = CARTESIAN_POINT ( 'NONE',  ( -3.679171394226034675, -2.494631558665844739, -0.3503314178412558211 ) ) ;
#6847 = CARTESIAN_POINT ( 'NONE',  ( 60.00000000000000000, 11.22300884646714891, 18.43052338851150651 ) ) ;
#6848 =( GEOMETRIC_REPRESENTATION_CONTEXT ( 3 ) GLOBAL_UNCERTAINTY_ASSIGNED_CONTEXT ( ( #1138 ) ) GLOBAL_UNIT_ASSIGNED_CONTEXT ( ( #18255, #16590, #19934 ) ) REPRESENTATION_CONTEXT ( 'NONE', 'WORKASPACE' ) );
#6849 = CARTESIAN_POINT ( 'NONE',  ( -3.458734125000000770, 0.000000000000000000, -2.012499998634403653 ) ) ;
#6850 = CARTESIAN_POINT ( 'NONE',  ( -2.828427124746188515, -2.828427124746190735, 13.12500000000001243 ) ) ;
#6851 = DIRECTION ( 'NONE',  ( 0.3373062947069096484, -0.9413949561959079615, -4.130810741450707148E-17 ) ) ;
#6852 = CARTESIAN_POINT ( 'NONE',  ( -3.458734124999998993, 1.432654583217640276, 17.37500000136559919 ) ) ;
#6853 = CARTESIAN_POINT ( 'NONE',  ( 4.000000000000000000, 4.898587196589412829E-16, -2.199999999999998845 ) ) ;
#6854 = EDGE_LOOP ( 'NONE', ( #3118, #4050, #6335, #20544 ) ) ;
#6855 = EDGE_CURVE ( 'NONE', #18435, #10807, #525, .T. ) ;
#6856 = CARTESIAN_POINT ( 'NONE',  ( -71.60000000109246798, 9.143825827087052716, 12.93301269999999192 ) ) ;
#6857 = EDGE_LOOP ( 'NONE', ( #19280, #11379, #8017, #6560, #3049 ) ) ;
#6858 = CARTESIAN_POINT ( 'NONE',  ( 53.87268183416157541, 7.926799079670491466, 12.83056023321021755 ) ) ;
#6859 = CARTESIAN_POINT ( 'NONE',  ( -67.40000000109247935, 7.933012699999995476, 15.85617417291294196 ) ) ;
#6860 = VECTOR ( 'NONE', #17708, 1000.000000000000114 ) ;
#6861 = CARTESIAN_POINT ( 'NONE',  ( -70.00000000000000000, -10.00000000000000000, 14.99999999999999645 ) ) ;
#6862 = EDGE_CURVE ( 'NONE', #11902, #18250, #18964, .T. ) ;
#6863 = VECTOR ( 'NONE', #13438, 1000.000000000000000 ) ;
#6864 = CARTESIAN_POINT ( 'NONE',  ( 3.458734125000001214, -1.432654583217639610, -1.824999998634404097 ) ) ;
#6865 = ORIENTED_EDGE ( 'NONE', *, *, #16227, .F. ) ;
#6866 = DIRECTION ( 'NONE',  ( 1.224646799147353207E-16, -0.000000000000000000, 1.000000000000000000 ) ) ;
#6867 = CIRCLE ( 'NONE', #1103, 2.500000000000000444 ) ;
#6868 = ORIENTED_EDGE ( 'NONE', *, *, #15214, .F. ) ;
#6869 = CARTESIAN_POINT ( 'NONE',  ( 0.000000000000000000, 2.357898499370431722, -2.818925648462311528E-15 ) ) ;
#6870 = ORIENTED_EDGE ( 'NONE', *, *, #22193, .T. ) ;
#6871 = EDGE_CURVE ( 'NONE', #5142, #21452, #14100, .T. ) ;
#6872 = CARTESIAN_POINT ( 'NONE',  ( 50.93981816583844591, 10.06805114094564857, 19.00000000000000000 ) ) ;
#6873 = PRODUCT_DEFINITION_FORMATION_WITH_SPECIFIED_SOURCE ( 'ANY', '', #11248, .NOT_KNOWN. ) ;
#6874 = CARTESIAN_POINT ( 'NONE',  ( -67.60000000218495586, 12.50000000000000000, 14.99999999999999645 ) ) ;
#6875 = VECTOR ( 'NONE', #10624, 1000.000000000000114 ) ;
#6876 = LINE ( 'NONE', #23034, #18635 ) ;
#6877 = DIRECTION ( 'NONE',  ( 0.000000000000000000, 0.000000000000000000, 1.000000000000000000 ) ) ;
#6878 = CARTESIAN_POINT ( 'NONE',  ( 1.432654583217643163, -3.458734124999999882, 14.00000000136560452 ) ) ;
#6879 = CARTESIAN_POINT ( 'NONE',  ( -4.000000000000000000, -1.656854249492383024, -2.512499997268812457 ) ) ;
#6880 = AXIS2_PLACEMENT_3D ( 'NONE', #12463, #14612, #3324 ) ;
#6881 = CARTESIAN_POINT ( 'NONE',  ( 56.71875000000000711, 13.00000000000000711, 16.24264068711927322 ) ) ;
#6882 = DIRECTION ( 'NONE',  ( 1.000000000000000000, -0.000000000000000000, -0.000000000000000000 ) ) ;
#6883 = CIRCLE ( 'NONE', #20250, 4.000000000000001776 ) ;
#6884 = CARTESIAN_POINT ( 'NONE',  ( 56.62500000000000000, 12.12132034355964727, 17.12132034355963484 ) ) ;
#6885 = EDGE_CURVE ( 'NONE', #10460, #2926, #20750, .T. ) ;
#6886 = CARTESIAN_POINT ( 'NONE',  ( 2.445694354108820079, 2.445694354108820523, 1.612500001365596125 ) ) ;
#6887 = CARTESIAN_POINT ( 'NONE',  ( 118.3095189484530181, 2.399706452296353820, 60.00000000000021316 ) ) ;
#6888 = LINE ( 'NONE', #10852, #16064 ) ;
#6889 = CIRCLE ( 'NONE', #18748, 2.500000000000000888 ) ;
#6890 = VERTEX_POINT ( 'NONE', #4471 ) ;
#6891 = CARTESIAN_POINT ( 'NONE',  ( 45.00000000000000000, 14.69846310392956745, 35.82846581308617573 ) ) ;
#6892 = LINE ( 'NONE', #12540, #21960 ) ;
#6893 = EDGE_LOOP ( 'NONE', ( #13893, #215, #13707, #15917 ) ) ;
#6894 = CARTESIAN_POINT ( 'NONE',  ( 58.03125000000000711, 11.24264068711929276, 18.00000000000000355 ) ) ;
#6895 = VECTOR ( 'NONE', #21679, 1000.000000000000000 ) ;
#6896 = CARTESIAN_POINT ( 'NONE',  ( -1.656854249492380804, 4.000000000000000000, -0.7624999972688126793 ) ) ;
#6897 = EDGE_CURVE ( 'NONE', #2984, #3455, #22788, .T. ) ;
#6898 = DIRECTION ( 'NONE',  ( 1.000000000000000000, -0.000000000000000000, -0.000000000000000000 ) ) ;
#6899 = VERTEX_POINT ( 'NONE', #6395 ) ;
#6900 = ORIENTED_EDGE ( 'NONE', *, *, #21808, .F. ) ;
#6901 = CARTESIAN_POINT ( 'NONE',  ( 3.250000000000001776, -5.629165124598848990, 1.734723475976807094E-15 ) ) ;
#6902 = CARTESIAN_POINT ( 'NONE',  ( -66.65000000000000568, 12.50000000000000000, 13.96446609406725692 ) ) ;
#6903 = ORIENTED_EDGE ( 'NONE', *, *, #1730, .F. ) ;
#6904 = ADVANCED_FACE ( 'NONE', ( #6282 ), #3375, .T. ) ;
#6905 = CARTESIAN_POINT ( 'NONE',  ( 4.140404888673277384, 2.228338276487440428, -3.686887068327033390 ) ) ;
#6906 = EDGE_CURVE ( 'NONE', #23355, #4600, #635, .T. ) ;
#6907 = CARTESIAN_POINT ( 'NONE',  ( -2.828427124746189403, 2.828427124746190291, 10.87500000000001066 ) ) ;
#6908 = VERTEX_POINT ( 'NONE', #15287 ) ;
#6909 = CARTESIAN_POINT ( 'NONE',  ( 4.000000000000000000, 0.7924765000094659007, -0.05906175389889852662 ) ) ;
#6910 = AXIS2_PLACEMENT_3D ( 'NONE', #9605, #16534, #9357 ) ;
#6911 = AXIS2_PLACEMENT_3D ( 'NONE', #22389, #3959, #11415 ) ;
#6912 = VECTOR ( 'NONE', #11295, 1000.000000000000000 ) ;
#6913 = CARTESIAN_POINT ( 'NONE',  ( 65.95000000109246230, 8.538419263543522320, 16.46158073645647235 ) ) ;
#6914 = CARTESIAN_POINT ( 'NONE',  ( 4.999999999999999112, 0.000000000000000000, 0.000000000000000000 ) ) ;
#6915 = MANIFOLD_SOLID_BREP ( 'Cavity1', #6264 ) ;
#6916 = LINE ( 'NONE', #61, #19119 ) ;
#6917 = CARTESIAN_POINT ( 'NONE',  ( 56.65856816583844591, 6.028187705514649330, 16.72490539043803182 ) ) ;
#6918 = CARTESIAN_POINT ( 'NONE',  ( 3.458734125000000326, 4.235727675282971730E-16, 3.237500001365597679 ) ) ;
#6919 = DIRECTION ( 'NONE',  ( 0.000000000000000000, -0.000000000000000000, 1.000000000000000000 ) ) ;
#6920 = CARTESIAN_POINT ( 'NONE',  ( 2.445694354108821411, 2.445694354108820523, 13.06250000136560452 ) ) ;
#6921 = CARTESIAN_POINT ( 'NONE',  ( 0.000000000000000000, 0.000000000000000000, 0.000000000000000000 ) ) ;
#6922 = DIRECTION ( 'NONE',  ( 0.000000000000000000, 0.000000000000000000, 1.000000000000000000 ) ) ;
#6923 = ORIENTED_EDGE ( 'NONE', *, *, #17089, .T. ) ;
#6924 = CARTESIAN_POINT ( 'NONE',  ( -0.3508590460142260725, 3.955718283038086369, 2.039999999999998259 ) ) ;
#6925 = DIRECTION ( 'NONE',  ( -7.087422195345011518E-32, -1.000000000000000000, -0.000000000000000000 ) ) ;
#6926 = DIRECTION ( 'NONE',  ( -0.9396926207859107594, -0.3420201433256623291, 1.540743955509804830E-32 ) ) ;
#6927 = AXIS2_PLACEMENT_3D ( 'NONE', #21646, #1291, #10328 ) ;
#6928 = ORIENTED_EDGE ( 'NONE', *, *, #6100, .F. ) ;
#6929 = CARTESIAN_POINT ( 'NONE',  ( 0.000000000000000000, 0.000000000000000000, 0.000000000000000000 ) ) ;
#6930 = DIRECTION ( 'NONE',  ( -1.000000000000000000, 0.000000000000000000, 0.000000000000000000 ) ) ;
#6931 = EDGE_CURVE ( 'NONE', #1543, #7617, #8371, .T. ) ;
#6932 = VERTEX_POINT ( 'NONE', #21208 ) ;
#6933 = EDGE_CURVE ( 'NONE', #15752, #21976, #6047, .T. ) ;
#6934 = DIRECTION ( 'NONE',  ( -1.000000000000000000, -0.000000000000000000, -0.000000000000000000 ) ) ;
#6935 = EDGE_LOOP ( 'NONE', ( #19729, #12947, #1368, #1018 ) ) ;
#6936 = CARTESIAN_POINT ( 'NONE',  ( -6.259644161404860030E-16, -4.618802153517027165, -3.433295621305388234 ) ) ;
#6937 = ORIENTED_EDGE ( 'NONE', *, *, #2903, .F. ) ;
#6938 = ADVANCED_FACE ( 'NONE', ( #17535 ), #22787, .T. ) ;
#6939 = CARTESIAN_POINT ( 'NONE',  ( 58.72106816583844591, 14.02818770551465377, 16.58880310854672757 ) ) ;
#6940 = CARTESIAN_POINT ( 'NONE',  ( 67.05000000218494449, 8.964466094067258695, 17.50000000000000355 ) ) ;
#6941 = FACE_OUTER_BOUND ( 'NONE', #21680, .T. ) ;
#6942 = CARTESIAN_POINT ( 'NONE',  ( 1.000350172342868515E-15, 3.864683531250000303, 10.67187500034141046 ) ) ;
#6943 = DIRECTION ( 'NONE',  ( -1.000000000000000000, 0.000000000000000000, 0.000000000000000000 ) ) ;
#6944 = ORIENTED_EDGE ( 'NONE', *, *, #21808, .T. ) ;
#6945 = AXIS2_PLACEMENT_3D ( 'NONE', #22238, #7317, #22112 ) ;
#6946 = DIRECTION ( 'NONE',  ( 0.000000000000000000, -0.000000000000000000, 1.000000000000000000 ) ) ;
#6947 = CARTESIAN_POINT ( 'NONE',  ( 35.00000000000000000, 4.500000000000001776, -20.00000000000000355 ) ) ;
#6948 = CARTESIAN_POINT ( 'NONE',  ( 67.95000000109247651, 11.46158073645647235, 13.53841926354352232 ) ) ;
#6949 = CARTESIAN_POINT ( 'NONE',  ( -1.432654583217639832, -3.458734125000000326, 17.87500000136560274 ) ) ;
#6950 = DIRECTION ( 'NONE',  ( 0.000000000000000000, 0.000000000000000000, -1.000000000000000000 ) ) ;
#6951 = FACE_OUTER_BOUND ( 'NONE', #1990, .T. ) ;
#6952 = EDGE_LOOP ( 'NONE', ( #6900, #12222, #23531, #19688 ) ) ;
#6953 = CARTESIAN_POINT ( 'NONE',  ( -2.724039609044899724, 2.140243184150454780, -3.295601554149323320 ) ) ;
#6954 = CARTESIAN_POINT ( 'NONE',  ( 55.03125000000000711, 11.24264068711929276, 18.00000000000000000 ) ) ;
#6955 = DIRECTION ( 'NONE',  ( -0.000000000000000000, -0.000000000000000000, 1.000000000000000000 ) ) ;
#6956 = VERTEX_POINT ( 'NONE', #20977 ) ;
#6957 = CARTESIAN_POINT ( 'NONE',  ( 36.99310306966726358, -11.25000000000000355, 5.000000000000079936 ) ) ;
#6958 = CARTESIAN_POINT ( 'NONE',  ( 6.353591512924457348E-16, -3.458734125000000326, -2.012499998634403653 ) ) ;
#6959 = DIRECTION ( 'NONE',  ( 0.000000000000000000, -1.000000000000000000, -0.000000000000000000 ) ) ;
#6960 = EDGE_LOOP ( 'NONE', ( #2435, #16090, #11270, #13105, #17113, #10008, #17939, #2509, #23416, #18931, #11003, #8122, #14786, #21542, #9440, #21180, #467, #9827, #2600 ) ) ;
#6961 = CARTESIAN_POINT ( 'NONE',  ( -4.024497503033519941, 2.323544716729375459, -3.572167766733379768 ) ) ;
#6962 = ORIENTED_EDGE ( 'NONE', *, *, #3510, .F. ) ;
#6963 = CARTESIAN_POINT ( 'NONE',  ( 9.920644283265380691E-16, 4.000000000000000000, 12.87500000273119660 ) ) ;
#6964 = ORIENTED_EDGE ( 'NONE', *, *, #13185, .T. ) ;
#6965 = CARTESIAN_POINT ( 'NONE',  ( 1.971781867644420635E-15, -4.000000000000000000, 18.25000000000001066 ) ) ;
#6966 = DIRECTION ( 'NONE',  ( 0.000000000000000000, 0.000000000000000000, 1.000000000000000000 ) ) ;
#6967 = FACE_OUTER_BOUND ( 'NONE', #23028, .T. ) ;
#6968 = CYLINDRICAL_SURFACE ( 'NONE', #18627, 5.000000000000000888 ) ;
#6969 = EDGE_CURVE ( 'NONE', #14005, #16753, #3019, .T. ) ;
#6970 = CARTESIAN_POINT ( 'NONE',  ( -70.84999999999998010, 11.03553390593273598, 17.50000000000000355 ) ) ;
#6971 = CARTESIAN_POINT ( 'NONE',  ( -65.00000000000000000, -10.00000000000000178, 17.49999999999999645 ) ) ;
#6972 = FACE_OUTER_BOUND ( 'NONE', #14656, .T. ) ;
#6973 = CARTESIAN_POINT ( 'NONE',  ( -1.432654583217640498, 3.458734125000000770, 0.8000000013655964581 ) ) ;
#6974 = CARTESIAN_POINT ( 'NONE',  ( 28.38725814676620018, -9.000000000000007105, 5.000000000000079936 ) ) ;
#6975 = CARTESIAN_POINT ( 'NONE',  ( -65.80000000218494449, 9.999999999999998224, 12.49999999999999289 ) ) ;
#6976 = CARTESIAN_POINT ( 'NONE',  ( 3.458734125000001214, 1.432654583217640498, 17.00000000136560629 ) ) ;
#6977 = DIRECTION ( 'NONE',  ( -0.8660254037844408170, 0.000000000000000000, 0.4999999999999961697 ) ) ;
#6978 = ORIENTED_EDGE ( 'NONE', *, *, #6763, .F. ) ;
#6979 = CARTESIAN_POINT ( 'NONE',  ( -70.75000000109247367, 8.538419263543524096, 13.53841926354352054 ) ) ;
#6980 = ORIENTED_EDGE ( 'NONE', *, *, #12634, .F. ) ;
#6981 = CARTESIAN_POINT ( 'NONE',  ( 52.56018183416157541, 7.000000000000000000, 14.93194885905437097 ) ) ;
#6982 = CARTESIAN_POINT ( 'NONE',  ( -67.05000000109247082, 12.06698730000000097, 14.99999999999999645 ) ) ;
#6983 = DIRECTION ( 'NONE',  ( 0.9942688056388265805, 0.1069090367253462820, 0.000000000000000000 ) ) ;
#6984 = CARTESIAN_POINT ( 'NONE',  ( -3.458734124999999882, -1.432654583217642275, -2.199999998634404097 ) ) ;
#6985 = ORIENTED_EDGE ( 'NONE', *, *, #8798, .F. ) ;
#6986 = DIRECTION ( 'NONE',  ( -0.000000000000000000, -0.000000000000000000, -1.000000000000000000 ) ) ;
#6987 = EDGE_LOOP ( 'NONE', ( #3555, #13979, #20675, #14722 ) ) ;
#6988 = CARTESIAN_POINT ( 'NONE',  ( 71.24999999999998579, 8.964466094067205404, 12.50000000000004263 ) ) ;
#6989 = VERTEX_POINT ( 'NONE', #4823 ) ;
#6990 = CARTESIAN_POINT ( 'NONE',  ( 54.40856816583843880, 12.97181229448534978, 13.68930817193506755 ) ) ;
#6991 = CARTESIAN_POINT ( 'NONE',  ( -66.70000000218495018, 11.76776695296636888, 13.23223304703362579 ) ) ;
#6992 =( BOUNDED_CURVE ( )  B_SPLINE_CURVE ( 2, ( #18269, #8968, #21967, #14710, #1510, #17926, #16370, #14239, #66 ),
 .UNSPECIFIED., .F., .F. ) 
 B_SPLINE_CURVE_WITH_KNOTS ( ( 3, 2, 2, 2, 3 ),
 ( 0.5999999999999999778, 0.6125000000000000444, 0.6250000000000000000, 0.6374999999999999556, 0.6500000000000000222 ),
 .UNSPECIFIED. ) 
 CURVE ( )  GEOMETRIC_REPRESENTATION_ITEM ( )  RATIONAL_B_SPLINE_CURVE ( ( 1.000000000000000000, 0.9238795325112867385, 1.000000000000000000, 0.9238795325112867385, 1.000000000000000000, 0.9238795325112867385, 1.000000000000000000, 0.9238795325112867385, 1.000000000000000000 ) ) 
 REPRESENTATION_ITEM ( '' )  );
#6993 = CARTESIAN_POINT ( 'NONE',  ( 72.50000000000000000, 9.999999999999998224, 17.49999999999999645 ) ) ;
#6994 = ADVANCED_FACE ( 'NONE', ( #4947 ), #13841, .F. ) ;
#6995 = LINE ( 'NONE', #23146, #11844 ) ;
#6996 = CARTESIAN_POINT ( 'NONE',  ( 2.445694354108822299, -2.445694354108820079, 14.06250000136560629 ) ) ;
#6997 = ADVANCED_FACE ( 'NONE', ( #23027 ), #9516, .T. ) ;
#6998 = CARTESIAN_POINT ( 'NONE',  ( -67.00000000218494733, 9.999999999999998224, 17.49999999999999645 ) ) ;
#6999 = CARTESIAN_POINT ( 'NONE',  ( 58.31250000000000000, 13.00000000000000000, 14.99999999999998757 ) ) ;
#7000 = CARTESIAN_POINT ( 'NONE',  ( 67.29999999999999716, 9.999999999999998224, 12.49999999999999289 ) ) ;
#7001 = CARTESIAN_POINT ( 'NONE',  ( 58.78125000000000711, 8.757359312880703683, 11.99999999999999822 ) ) ;
#7002 = CARTESIAN_POINT ( 'NONE',  ( -2.117863837641485618E-16, 3.458734125000000770, -3.262499998634402765 ) ) ;
#7003 = CARTESIAN_POINT ( 'NONE',  ( -12.00000000000000000, 1.469576158976823947E-15, 1.469576158976823947E-15 ) ) ;
#7004 = CIRCLE ( 'NONE', #8935, 11.00000000000000000 ) ;
#7005 = EDGE_CURVE ( 'NONE', #11553, #5706, #8203, .T. ) ;
#7006 = CARTESIAN_POINT ( 'NONE',  ( 70.50000000218494733, 8.232233047033629347, 13.23223304703362402 ) ) ;
#7007 = ORIENTED_EDGE ( 'NONE', *, *, #5834, .F. ) ;
#7008 = CARTESIAN_POINT ( 'NONE',  ( -4.000000000000000000, -2.309401076758515803, -0.4999999999999995559 ) ) ;
#7009 = CARTESIAN_POINT ( 'NONE',  ( -1.274258131565027874, -3.883108878240886241, -3.220599429844051009 ) ) ;
#7010 = VERTEX_POINT ( 'NONE', #1102 ) ;
#7011 = CARTESIAN_POINT ( 'NONE',  ( 58.31250000000000000, 13.00000000000000000, 14.99999999999998757 ) ) ;
#7012 = CARTESIAN_POINT ( 'NONE',  ( -2.449293598294706907E-16, 4.000000000000000000, -0.8249999972688125682 ) ) ;
#7013 = VECTOR ( 'NONE', #4438, 1000.000000000000000 ) ;
#7014 = DIRECTION ( 'NONE',  ( 0.000000000000000000, 0.000000000000000000, 1.000000000000000000 ) ) ;
#7015 = EDGE_LOOP ( 'NONE', ( #23088, #10189, #16447, #3464 ) ) ;
#7016 = CARTESIAN_POINT ( 'NONE',  ( -2.828427124746188515, -2.828427124746190735, 17.12500000000001066 ) ) ;
#7017 = ORIENTED_EDGE ( 'NONE', *, *, #8863, .T. ) ;
#7018 =( NAMED_UNIT ( * ) SI_UNIT ( $, .STERADIAN. ) SOLID_ANGLE_UNIT ( ) );
#7019 = LINE ( 'NONE', #8480, #16009 ) ;
#7020 = ORIENTED_EDGE ( 'NONE', *, *, #10964, .F. ) ;
#7021 = FACE_BOUND ( 'NONE', #21632, .T. ) ;
#7022 = CARTESIAN_POINT ( 'NONE',  ( 0.000000000000000000, 0.000000000000000000, -3.674599999999999866 ) ) ;
#7023 = EDGE_CURVE ( 'NONE', #22879, #15720, #15973, .T. ) ;
#7024 = ORIENTED_EDGE ( 'NONE', *, *, #18730, .F. ) ;
#7025 = CARTESIAN_POINT ( 'NONE',  ( 65.85000000109248219, 7.933012699999995476, 14.99999999999999645 ) ) ;
#7026 = VECTOR ( 'NONE', #12477, 1000.000000000000000 ) ;
#7027 = ADVANCED_FACE ( 'NONE', ( #2675 ), #17420, .F. ) ;
#7028 = CARTESIAN_POINT ( 'NONE',  ( 70.74999999999998579, 12.50000000000000000, 16.03553390593273420 ) ) ;
#7029 = CIRCLE ( 'NONE', #4727, 2.649999999999992806 ) ;
#7030 = EDGE_CURVE ( 'NONE', #4263, #5746, #17765, .T. ) ;
#7031 = CARTESIAN_POINT ( 'NONE',  ( -65.70000000218495018, 8.232233047033629347, 13.23223304703362402 ) ) ;
#7032 = CARTESIAN_POINT ( 'NONE',  ( 0.000000000000000000, 0.000000000000000000, 0.000000000000000000 ) ) ;
#7033 = CARTESIAN_POINT ( 'NONE',  ( 57.68981816583843170, 9.931948859054346102, 10.99999999999999467 ) ) ;
#7034 = CARTESIAN_POINT ( 'NONE',  ( -3.458734124999999882, -1.432654583217642497, 3.800000001365595459 ) ) ;
#7035 = EDGE_CURVE ( 'NONE', #16269, #18845, #12197, .T. ) ;
#7036 = CARTESIAN_POINT ( 'NONE',  ( -2.445694354108819191, 2.445694354108820523, 16.31250000136560629 ) ) ;
#7037 = CARTESIAN_POINT ( 'NONE',  ( -2.828427124746188515, -2.828427124746190735, 18.25000000273119483 ) ) ;
#7038 = EDGE_CURVE ( 'NONE', #19003, #892, #6750, .T. ) ;
#7039 = CARTESIAN_POINT ( 'NONE',  ( -70.50000000218494733, 8.232233047033629347, 13.23223304703362402 ) ) ;
#7040 = ORIENTED_EDGE ( 'NONE', *, *, #12050, .F. ) ;
#7041 = CYLINDRICAL_SURFACE ( 'NONE', #1914, 6.000000000000000888 ) ;
#7042 = DIRECTION ( 'NONE',  ( -1.000000000000000000, 0.000000000000000000, 0.000000000000000000 ) ) ;
#7043 = DIRECTION ( 'NONE',  ( 1.000000000000000000, 0.000000000000000000, 0.000000000000000000 ) ) ;
#7044 = EDGE_LOOP ( 'NONE', ( #9268, #14051, #19571, #14545 ) ) ;
#7045 = DIRECTION ( 'NONE',  ( 1.000000000000000000, 0.000000000000000000, -0.000000000000000000 ) ) ;
#7046 = ORIENTED_EDGE ( 'NONE', *, *, #8046, .F. ) ;
#7047 = CARTESIAN_POINT ( 'NONE',  ( -1.489200000000000301, 0.000000000000000000, 0.000000000000000000 ) ) ;
#7048 = VERTEX_POINT ( 'NONE', #21326 ) ;
#7049 = CARTESIAN_POINT ( 'NONE',  ( 66.15000000218496723, 11.03553390593268624, 17.50000000000005329 ) ) ;
#7050 = VERTEX_POINT ( 'NONE', #10484 ) ;
#7051 = CARTESIAN_POINT ( 'NONE',  ( 58.43981816583843170, 10.06805114094564857, 19.00000000000000000 ) ) ;
#7052 = CARTESIAN_POINT ( 'NONE',  ( 68.05000000218494449, 7.499999999999995559, 13.96446609406725692 ) ) ;
#7053 = VECTOR ( 'NONE', #15900, 1000.000000000000000 ) ;
#7054 = CARTESIAN_POINT ( 'NONE',  ( 0.000000000000000000, 9.314797388894909602, -1.239665997526783858 ) ) ;
#7055 = PLANE ( 'NONE',  #16743 ) ;
#7056 = ADVANCED_FACE ( 'NONE', ( #12042 ), #1334, .T. ) ;
#7057 = LINE ( 'NONE', #14376, #4552 ) ;
#7058 = EDGE_LOOP ( 'NONE', ( #14443, #1783, #22944, #17657 ) ) ;
#7059 = DIRECTION ( 'NONE',  ( 7.087422195345011518E-32, 1.000000000000000000, -0.000000000000000000 ) ) ;
#7060 = EDGE_CURVE ( 'NONE', #1856, #6742, #19082, .T. ) ;
#7061 = CARTESIAN_POINT ( 'NONE',  ( 60.06018183416157541, 5.999999999999996447, 14.93194885905437808 ) ) ;
#7062 = DIRECTION ( 'NONE',  ( 7.087422195345011518E-32, 1.000000000000000000, -0.000000000000000000 ) ) ;
#7063 = CARTESIAN_POINT ( 'NONE',  ( 65.85000000109246798, 9.999999999999998224, 17.06698730000000097 ) ) ;
#7064 = CARTESIAN_POINT ( 'NONE',  ( -69.25000000000000000, 11.03553390593269157, 17.50000000000004619 ) ) ;
#7065 = EDGE_CURVE ( 'NONE', #23109, #6666, #12592, .T. ) ;
#7066 = LINE ( 'NONE', #23343, #22983 ) ;
#7067 = ORIENTED_EDGE ( 'NONE', *, *, #14508, .F. ) ;
#7068 = DIRECTION ( 'NONE',  ( -1.000000000000000000, 0.000000000000000000, 0.000000000000000000 ) ) ;
#7069 = VECTOR ( 'NONE', #7777, 1000.000000000000000 ) ;
#7070 = CARTESIAN_POINT ( 'NONE',  ( 59.71875000000000711, 13.00000000000000533, 16.24264068711927322 ) ) ;
#7071 = LINE ( 'NONE', #4909, #20009 ) ;
#7072 = CARTESIAN_POINT ( 'NONE',  ( 1.236993788156008760E-15, 0.000000000000000000, -20.00000000000000000 ) ) ;
#7073 = ORIENTED_EDGE ( 'NONE', *, *, #3664, .F. ) ;
#7074 = DIRECTION ( 'NONE',  ( 0.000000000000000000, 0.000000000000000000, 1.000000000000000000 ) ) ;
#7075 = CARTESIAN_POINT ( 'NONE',  ( -1.432654583217640942, -3.458734124999999882, -2.074999998634404097 ) ) ;
#7076 = DIRECTION ( 'NONE',  ( 0.9413949561959079615, 0.3373062947069096484, -0.000000000000000000 ) ) ;
#7077 = CIRCLE ( 'NONE', #10154, 2.649999999999989253 ) ;
#7078 = VECTOR ( 'NONE', #21167, 1000.000000000000000 ) ;
#7079 = VERTEX_POINT ( 'NONE', #22907 ) ;
#7080 = FACE_OUTER_BOUND ( 'NONE', #23387, .T. ) ;
#7081 = EDGE_LOOP ( 'NONE', ( #8391, #1153, #1458, #12612 ) ) ;
#7082 = CARTESIAN_POINT ( 'NONE',  ( -2.828427124746189403, 2.828427124746190291, 18.87500000000001066 ) ) ;
#7083 = CARTESIAN_POINT ( 'NONE',  ( -3.999999999999999112, 1.656854249492380804, 18.93750000000000711 ) ) ;
#7084 = CARTESIAN_POINT ( 'NONE',  ( -4.000000000000000000, 0.7924765000094600165, -0.05906175389889745803 ) ) ;
#7085 = LINE ( 'NONE', #14403, #9564 ) ;
#7086 = SURFACE_SIDE_STYLE ('',( #12964 ) ) ;
#7087 = CARTESIAN_POINT ( 'NONE',  ( 4.999999999999999112, 4.472189673936902921, -8.264486777890061475 ) ) ;
#7088 = AXIS2_PLACEMENT_3D ( 'NONE', #9350, #341, #18667 ) ;
#7089 = AXIS2_PLACEMENT_3D ( 'NONE', #18539, #101, #7433 ) ;
#7090 = CARTESIAN_POINT ( 'NONE',  ( -66.69999999999998863, 12.50000000000000000, 14.99999999999999645 ) ) ;
#7091 = AXIS2_PLACEMENT_3D ( 'NONE', #12907, #21856, #14470 ) ;
#7092 = DIRECTION ( 'NONE',  ( 0.000000000000000000, 0.000000000000000000, -1.000000000000000000 ) ) ;
#7093 = EDGE_CURVE ( 'NONE', #11644, #17824, #19796, .T. ) ;
#7094 = CARTESIAN_POINT ( 'NONE',  ( 60.00000000000004263, 12.51911211317366046, 16.88872345643414263 ) ) ;
#7095 = LINE ( 'NONE', #2147, #13416 ) ;
#7096 = CARTESIAN_POINT ( 'NONE',  ( -2.449293598294706907E-16, 4.000000000000000000, 4.049999999999999822 ) ) ;
#7097 = CARTESIAN_POINT ( 'NONE',  ( -66.35000000109246798, 11.46158073645647235, 13.53841926354352232 ) ) ;
#7098 = DIRECTION ( 'NONE',  ( -1.000000000000000000, 0.000000000000000000, 0.000000000000000000 ) ) ;
#7099 = CARTESIAN_POINT ( 'NONE',  ( -2.445694354108818303, -2.445694354108820523, 16.56250000136560629 ) ) ;
#7100 = DIRECTION ( 'NONE',  ( 7.087422195345011518E-32, 1.000000000000000000, -0.000000000000000000 ) ) ;
#7101 = VERTEX_POINT ( 'NONE', #4710 ) ;
#7102 = CARTESIAN_POINT ( 'NONE',  ( -71.05000000109247082, 12.06698730000000097, 14.99999999999999645 ) ) ;
#7103 = ORIENTED_EDGE ( 'NONE', *, *, #19938, .T. ) ;
#7104 = CARTESIAN_POINT ( 'NONE',  ( 53.87268183416157541, 7.219692298483935566, 12.12345345202367675 ) ) ;
#7105 = CARTESIAN_POINT ( 'NONE',  ( -66.65000000109247935, 7.933012699999995476, 14.99999999999999645 ) ) ;
#7106 = DIRECTION ( 'NONE',  ( 1.000000000000000000, 1.232595164407830672E-32, 2.052683297350805345E-48 ) ) ;
#7107 = CARTESIAN_POINT ( 'NONE',  ( 6.353591512924457348E-16, -3.458734125000000326, -2.012499998634403653 ) ) ;
#7108 = ORIENTED_EDGE ( 'NONE', *, *, #10504, .F. ) ;
#7109 = CARTESIAN_POINT ( 'NONE',  ( 19.56809120928344825, -8.974600000000002353, 5.000000000000079936 ) ) ;
#7110 = VECTOR ( 'NONE', #4446, 1000.000000000000000 ) ;
#7111 = ORIENTED_EDGE ( 'NONE', *, *, #15350, .T. ) ;
#7112 = CIRCLE ( 'NONE', #7877, 5.560781378645573980 ) ;
#7113 = DIRECTION ( 'NONE',  ( -1.000000000000000000, -0.000000000000000000, -0.000000000000000000 ) ) ;
#7114 = VERTEX_POINT ( 'NONE', #2010 ) ;
#7115 = CARTESIAN_POINT ( 'NONE',  ( 50.00231816583843170, 12.07320092032949610, 12.83056023321021044 ) ) ;
#7116 = CARTESIAN_POINT ( 'NONE',  ( -70.00000000109248788, 9.143825827087050939, 12.93301269999999370 ) ) ;
#7117 = AXIS2_PLACEMENT_3D ( 'NONE', #6094, #9948, #22613 ) ;
#7118 = VECTOR ( 'NONE', #9845, 1000.000000000000114 ) ;
#7119 = CARTESIAN_POINT ( 'NONE',  ( -70.90000000109245093, 7.933012699999995476, 14.14382582708705094 ) ) ;
#7120 = CARTESIAN_POINT ( 'NONE',  ( 3.458734125000001658, 4.235727675282972223E-16, 17.18750000136560629 ) ) ;
#7121 = DIRECTION ( 'NONE',  ( 0.000000000000000000, 0.000000000000000000, 1.000000000000000000 ) ) ;
#7122 = CARTESIAN_POINT ( 'NONE',  ( 53.06250000000000711, 6.999999999999997335, 15.00000000000000533 ) ) ;
#7123 = CARTESIAN_POINT ( 'NONE',  ( 24.42673246966726452, -11.25000000000000355, 5.000000000000079936 ) ) ;
#7124 = AXIS2_PLACEMENT_3D ( 'NONE', #12368, #19631, #1194 ) ;
#7125 = CARTESIAN_POINT ( 'NONE',  ( 58.40625000000000711, 12.99999999999999645, 13.75735931288070191 ) ) ;
#7126 = CARTESIAN_POINT ( 'NONE',  ( 2.445694354108820079, 2.445694354108820523, -2.387499998634403653 ) ) ;
#7127 = CARTESIAN_POINT ( 'NONE',  ( -1.313672045791830501, -3.207643946584868289, 2.039999999999997815 ) ) ;
#7128 = DIRECTION ( 'NONE',  ( -1.000000000000000000, 0.000000000000000000, -0.000000000000000000 ) ) ;
#7129 = ORIENTED_EDGE ( 'NONE', *, *, #17970, .T. ) ;
#7130 = CARTESIAN_POINT ( 'NONE',  ( 4.999999999999999112, 8.152713396088763886, 3.174628368996105010 ) ) ;
#7131 = DIRECTION ( 'NONE',  ( 1.000000000000000000, -0.000000000000000000, -0.000000000000000000 ) ) ;
#7132 = ORIENTED_EDGE ( 'NONE', *, *, #22666, .T. ) ;
#7133 = CARTESIAN_POINT ( 'NONE',  ( 52.87500000000000711, 7.878679656440349177, 12.87867965644035984 ) ) ;
#7134 = CARTESIAN_POINT ( 'NONE',  ( -1.656854249492381248, -3.999999999999999112, 0.6125000027311866546 ) ) ;
#7135 = DIRECTION ( 'NONE',  ( -0.9396926207859107594, -0.3420201433256623291, 1.540743955509804830E-32 ) ) ;
#7136 = ORIENTED_EDGE ( 'NONE', *, *, #11264, .T. ) ;
#7137 = CARTESIAN_POINT ( 'NONE',  ( 1.971781867644420635E-15, -4.000000000000000000, 17.25000000000001066 ) ) ;
#7138 = ORIENTED_EDGE ( 'NONE', *, *, #17973, .F. ) ;
#7139 = EDGE_CURVE ( 'NONE', #22026, #3850, #11159, .T. ) ;
#7140 =( NAMED_UNIT ( * ) PLANE_ANGLE_UNIT ( ) SI_UNIT ( $, .RADIAN. ) );
#7141 =( BOUNDED_SURFACE ( )  B_SPLINE_SURFACE ( 3, 2, ( 
 ( #22945, #6905, #4984 ),
 ( #11964, #15786, #8836 ),
 ( #22818, #15894, #4858 ),
 ( #8353, #6431, #17459 ),
 ( #3173, #23057, #19465 ),
 ( #1022, #10519, #17572 ) ),
 .UNSPECIFIED., .F., .F., .T. ) 
 B_SPLINE_SURFACE_WITH_KNOTS ( ( 4, 2, 4 ),
 ( 3, 3 ),
 ( 0.02032853247518126225, 0.02278863295364821212, 0.02524873343211516200 ),
 ( 0.000000000000000000, 1.000000000000000000 ),
 .UNSPECIFIED. ) 
 GEOMETRIC_REPRESENTATION_ITEM ( )  RATIONAL_B_SPLINE_SURFACE ( (
 ( 1.000000000000000000, 0.8047781615896835161, 1.000000000000000000),
 ( 1.000000000000000000, 0.8123767586291043008, 1.000000000000000000),
 ( 1.000000000000000000, 0.8190662415562011134, 1.000000000000000000),
 ( 1.000000000000000000, 0.8192361015671398849, 1.000000000000000000),
 ( 1.000000000000000000, 0.8126135807102121689, 1.000000000000000000),
 ( 1.000000000000000000, 0.8047712338318585568, 1.000000000000000000) ) ) 
 REPRESENTATION_ITEM ( '' )  SURFACE ( )  );
#7142 = DIRECTION ( 'NONE',  ( 0.000000000000000000, 0.000000000000000000, -1.000000000000000000 ) ) ;
#7143 = ORIENTED_EDGE ( 'NONE', *, *, #15201, .F. ) ;
#7144 = CARTESIAN_POINT ( 'NONE',  ( 4.999999999999999112, 8.264486777890107660, 4.472189673936815879 ) ) ;
#7145 = CARTESIAN_POINT ( 'NONE',  ( 44.89825008461777855, -9.517000605182268202, 10.48564008399537428 ) ) ;
#7146 = VERTEX_POINT ( 'NONE', #2254 ) ;
#7147 = EDGE_CURVE ( 'NONE', #11298, #20551, #3420, .T. ) ;
#7148 = CARTESIAN_POINT ( 'NONE',  ( 66.30000000109247082, 12.06698730000000275, 15.85617417291294196 ) ) ;
#7149 = CARTESIAN_POINT ( 'NONE',  ( 70.84999999999998010, 11.03553390593273598, 17.50000000000000355 ) ) ;
#7150 = CARTESIAN_POINT ( 'NONE',  ( 11.86036186966726191, -11.25000000000000355, 5.000000000000079936 ) ) ;
#7151 = CARTESIAN_POINT ( 'NONE',  ( 69.49999999999998579, 7.499999999999996447, 14.99999999999999645 ) ) ;
#7152 = CARTESIAN_POINT ( 'NONE',  ( 58.25231816583843170, 7.219692298483957771, 17.87654654797633924 ) ) ;
#7153 = CARTESIAN_POINT ( 'NONE',  ( -3.458734124999999882, -1.432654583217642497, 0.8000000013655964581 ) ) ;
#7154 = CARTESIAN_POINT ( 'NONE',  ( -2.000000000000001776, 0.000000000000000000, -8.800000000000022027 ) ) ;
#7155 = CARTESIAN_POINT ( 'NONE',  ( 1.872352939448454495E-15, -3.458734125000000326, 13.68750000136560629 ) ) ;
#7156 = DIRECTION ( 'NONE',  ( 0.000000000000000000, 0.000000000000000000, -1.000000000000000000 ) ) ;
#7157 = CARTESIAN_POINT ( 'NONE',  ( 65.00000000000000000, -9.999999999999998224, 24.99999999999999645 ) ) ;
#7158 = ORIENTED_EDGE ( 'NONE', *, *, #441, .F. ) ;
#7159 = LINE ( 'NONE', #19949, #6142 ) ;
#7160 = CARTESIAN_POINT ( 'NONE',  ( -6.500000000000001776, 0.6345343291280540754, -3.700000000000001066 ) ) ;
#7161 = DIRECTION ( 'NONE',  ( -0.000000000000000000, -0.000000000000000000, 1.000000000000000000 ) ) ;
#7162 = ORIENTED_EDGE ( 'NONE', *, *, #12594, .F. ) ;
#7163 = ORIENTED_EDGE ( 'NONE', *, *, #19059, .T. ) ;
#7164 = EDGE_CURVE ( 'NONE', #12363, #19458, #20214, .T. ) ;
#7165 = DIRECTION ( 'NONE',  ( 0.000000000000000000, 0.000000000000000000, -1.000000000000000000 ) ) ;
#7166 = ADVANCED_FACE ( 'NONE', ( #23384 ), #21565, .T. ) ;
#7167 = VERTEX_POINT ( 'NONE', #16098 ) ;
#7168 = CARTESIAN_POINT ( 'NONE',  ( 57.09375000000000711, 11.65685424949236015, 10.99999999999998579 ) ) ;
#7169 = ORIENTED_EDGE ( 'NONE', *, *, #18593, .F. ) ;
#7170 = CARTESIAN_POINT ( 'NONE',  ( 18.14354716966726144, -11.25000000000000355, 5.000000000000079936 ) ) ;
#7171 = EDGE_LOOP ( 'NONE', ( #11813, #12826, #14488, #10345 ) ) ;
#7172 = AXIS2_PLACEMENT_3D ( 'NONE', #2792, #20753, #18740 ) ;
#7173 = CARTESIAN_POINT ( 'NONE',  ( 52.21875000000002842, 14.00000000000000888, 16.65685424949235482 ) ) ;
#7174 = ADVANCED_FACE ( 'NONE', ( #14426 ), #18001, .T. ) ;
#7175 = CARTESIAN_POINT ( 'NONE',  ( 69.10000000218495586, 11.76776695296636888, 13.23223304703362579 ) ) ;
#7176 =( BOUNDED_CURVE ( )  B_SPLINE_CURVE ( 1, ( #10997, #10779 ),
 .UNSPECIFIED., .F., .F. ) 
 B_SPLINE_CURVE_WITH_KNOTS ( ( 2, 2 ),
 ( 0.000000000000000000, 1.000000000000000000 ),
 .UNSPECIFIED. ) 
 CURVE ( )  GEOMETRIC_REPRESENTATION_ITEM ( )  RATIONAL_B_SPLINE_CURVE ( ( 0.9841097943611589738, 0.9841097943611589738 ) ) 
 REPRESENTATION_ITEM ( '' )  );
#7177 = AXIS2_PLACEMENT_3D ( 'NONE', #5670, #10820, #14529 ) ;
#7178 = FACE_OUTER_BOUND ( 'NONE', #4320, .T. ) ;
#7179 = CARTESIAN_POINT ( 'NONE',  ( -68.59999999999999432, 8.232233047033627571, 16.76776695296636532 ) ) ;
#7180 = CARTESIAN_POINT ( 'NONE',  ( 50.00000000000000000, 15.00000000000001954, 10.00000000000008882 ) ) ;
#7181 = ORIENTED_EDGE ( 'NONE', *, *, #11967, .F. ) ;
#7182 = CARTESIAN_POINT ( 'NONE',  ( 4.000000000000001776, -1.656854249492379694, 17.56250000273119838 ) ) ;
#7183 =( REPRESENTATION_RELATIONSHIP ('NONE','NONE', #8403, #15757 ) REPRESENTATION_RELATIONSHIP_WITH_TRANSFORMATION ( #10340 )SHAPE_REPRESENTATION_RELATIONSHIP( ) );
#7184 = CARTESIAN_POINT ( 'NONE',  ( -6.500000000000000000, 0.000000000000000000, 1.734723475976807094E-15 ) ) ;
#7185 = CARTESIAN_POINT ( 'NONE',  ( 59.02893183416158251, 11.58880310854676132, 19.02818770551463956 ) ) ;
#7186 = CARTESIAN_POINT ( 'NONE',  ( 2.813044857425830880, -2.271656904766521823, 2.040000000000001368 ) ) ;
#7187 = CARTESIAN_POINT ( 'NONE',  ( 67.00000000109247367, 9.143825827087050939, 12.93301269999999370 ) ) ;
#7188 = VECTOR ( 'NONE', #21975, 1000.000000000000000 ) ;
#7189 = CARTESIAN_POINT ( 'NONE',  ( -67.95000000000001705, 7.499999999999996447, 13.96446609406725514 ) ) ;
#7190 = AXIS2_PLACEMENT_3D ( 'NONE', #19015, #13538, #11523 ) ;
#7191 = CARTESIAN_POINT ( 'NONE',  ( -0.7060087303327398089, -11.25000000000000355, 10.00000000000008882 ) ) ;
#7192 = EDGE_LOOP ( 'NONE', ( #10329, #23299, #13982, #13401 ) ) ;
#7193 = DIRECTION ( 'NONE',  ( 0.000000000000000000, 0.000000000000000000, 1.000000000000000000 ) ) ;
#7194 = CARTESIAN_POINT ( 'NONE',  ( 54.37500000000000711, 7.878679656440349177, 12.87867965644035984 ) ) ;
#7195 = ADVANCED_FACE ( 'NONE', ( #21690 ), #16890, .F. ) ;
#7196 = FACE_OUTER_BOUND ( 'NONE', #2731, .T. ) ;
#7197 = LINE ( 'NONE', #23585, #6160 ) ;
#7198 = ORIENTED_EDGE ( 'NONE', *, *, #20433, .T. ) ;
#7199 = CARTESIAN_POINT ( 'NONE',  ( 0.000000000000000000, -8.461683424509331530, 2.223716399045538861 ) ) ;
#7200 = CARTESIAN_POINT ( 'NONE',  ( -2.117863837641485618E-16, 3.458734125000000326, -0.5124999986344038749 ) ) ;
#7201 = PLANE ( 'NONE',  #8613 ) ;
#7202 = EDGE_CURVE ( 'NONE', #7460, #18054, #13186, .T. ) ;
#7203 = ORIENTED_EDGE ( 'NONE', *, *, #16552, .T. ) ;
#7204 = CARTESIAN_POINT ( 'NONE',  ( 2.682243648011666703, 3.070208061305304881, -0.04852650426601266831 ) ) ;
#7205 = ORIENTED_EDGE ( 'NONE', *, *, #4249, .F. ) ;
#7206 = VECTOR ( 'NONE', #1307, 1000.000000000000114 ) ;
#7207 = LINE ( 'NONE', #12253, #20170 ) ;
#7208 = CARTESIAN_POINT ( 'NONE',  ( 9.920644283265380691E-16, 4.000000000000000000, 16.75000000000001066 ) ) ;
#7209 = EDGE_CURVE ( 'NONE', #12336, #2236, #8334, .T. ) ;
#7210 = CARTESIAN_POINT ( 'NONE',  ( -6.259644161404860030E-16, -4.618802153517027165, -5.000000000000000000 ) ) ;
#7211 = CIRCLE ( 'NONE', #20558, 0.5000000000000006661 ) ;
#7212 = EDGE_CURVE ( 'NONE', #16384, #19904, #13706, .T. ) ;
#7213 = AXIS2_PLACEMENT_3D ( 'NONE', #13368, #13716, #13488 ) ;
#7214 = DIRECTION ( 'NONE',  ( -1.000000000000000000, 0.000000000000000000, 0.000000000000000000 ) ) ;
#7215 = DIRECTION ( 'NONE',  ( -0.000000000000000000, -0.000000000000000000, -1.000000000000000000 ) ) ;
#7216 = CARTESIAN_POINT ( 'NONE',  ( 4.999999999999999112, -1.975651141462163363, -10.82112760146738495 ) ) ;
#7217 = CARTESIAN_POINT ( 'NONE',  ( -66.15000000000000568, 8.964466094067258695, 17.50000000000000355 ) ) ;
#7218 = CARTESIAN_POINT ( 'NONE',  ( 4.999999999999999112, 8.152713396088806519, -3.174628368995992655 ) ) ;
#7219 = CARTESIAN_POINT ( 'NONE',  ( 1.872352939448454495E-15, -3.458734125000000326, 16.68750000136560629 ) ) ;
#7220 = CARTESIAN_POINT ( 'NONE',  ( -27.50000000000000711, 4.500000000000003553, -33.66025403784446723 ) ) ;
#7221 = CIRCLE ( 'NONE', #3365, 8.265000000000021885 ) ;
#7222 = CARTESIAN_POINT ( 'NONE',  ( -2.828427124746189403, -2.828427124746190735, 5.425000000000000711 ) ) ;
#7223 = CARTESIAN_POINT ( 'NONE',  ( 3.458734125000002102, -1.432654583217639610, 18.87500000136560274 ) ) ;
#7224 = DIRECTION ( 'NONE',  ( 0.000000000000000000, 0.000000000000000000, -1.000000000000000000 ) ) ;
#7225 = AXIS2_PLACEMENT_3D ( 'NONE', #6640, #991, #8800 ) ;
#7226 = ORIENTED_EDGE ( 'NONE', *, *, #20063, .T. ) ;
#7227 = VECTOR ( 'NONE', #5855, 1000.000000000000000 ) ;
#7228 = CARTESIAN_POINT ( 'NONE',  ( -70.20000000109246230, 12.06698729999999919, 14.14382582708705094 ) ) ;
#7229 = VERTEX_POINT ( 'NONE', #12951 ) ;
#7230 = CARTESIAN_POINT ( 'NONE',  ( 52.65393183416158251, 5.971812294485358663, 16.58880310854675599 ) ) ;
#7231 = CARTESIAN_POINT ( 'NONE',  ( -65.85000000109248219, 7.933012699999995476, 14.99999999999999645 ) ) ;
#7232 = DIRECTION ( 'NONE',  ( -0.9413949561959080725, -0.3373062947069098150, 0.000000000000000000 ) ) ;
#7233 = DIRECTION ( 'NONE',  ( -0.000000000000000000, -0.000000000000000000, 1.000000000000000000 ) ) ;
#7234 = EDGE_LOOP ( 'NONE', ( #9009, #13187, #22087, #14250 ) ) ;
#7235 = ORIENTED_EDGE ( 'NONE', *, *, #1162, .T. ) ;
#7236 = CARTESIAN_POINT ( 'NONE',  ( -1.432654583217639166, 3.458734125000000770, 19.50000000136560629 ) ) ;
#7237 = EDGE_CURVE ( 'NONE', #7712, #23556, #18432, .T. ) ;
#7238 = CARTESIAN_POINT ( 'NONE',  ( 54.31481816583844591, 12.99999999999999822, 14.93194885905435676 ) ) ;
#7239 = EDGE_CURVE ( 'NONE', #21282, #21603, #18873, .T. ) ;
#7240 = VECTOR ( 'NONE', #9478, 1000.000000000000000 ) ;
#7241 = CARTESIAN_POINT ( 'NONE',  ( -71.90000000109247935, 12.06698730000000275, 15.85617417291294196 ) ) ;
#7242 = CARTESIAN_POINT ( 'NONE',  ( -71.35000000109246798, 11.46158073645647235, 16.46158073645647235 ) ) ;
#7243 = VECTOR ( 'NONE', #19957, 1000.000000000000000 ) ;
#7244 = CARTESIAN_POINT ( 'NONE',  ( -3.458734124999999437, 1.432654583217640498, 14.62500000136560452 ) ) ;
#7245 = CARTESIAN_POINT ( 'NONE',  ( 72.50000000000000000, 9.999999999999998224, 12.49999999999999289 ) ) ;
#7246 = CARTESIAN_POINT ( 'NONE',  ( 52.31250000000000711, 13.00000000000000000, 14.99999999999998757 ) ) ;
#7247 = DIRECTION ( 'NONE',  ( 0.000000000000000000, 0.000000000000000000, 1.000000000000000000 ) ) ;
#7248 = CARTESIAN_POINT ( 'NONE',  ( 52.96875000000000000, 6.999999999999992895, 13.75735931288071967 ) ) ;
#7249 = CARTESIAN_POINT ( 'NONE',  ( 0.000000000000000000, 0.000000000000000000, 0.000000000000000000 ) ) ;
#7250 = AXIS2_PLACEMENT_3D ( 'NONE', #12352, #19614, #10559 ) ;
#7251 = LINE ( 'NONE', #41, #18735 ) ;
#7252 = AXIS2_PLACEMENT_3D ( 'NONE', #12112, #6816, #11883 ) ;
#7253 = EDGE_LOOP ( 'NONE', ( #22162, #6387 ) ) ;
#7254 = FACE_OUTER_BOUND ( 'NONE', #18173, .T. ) ;
#7255 = DIRECTION ( 'NONE',  ( -1.000000000000000000, -0.000000000000000000, -0.000000000000000000 ) ) ;
#7256 = ORIENTED_EDGE ( 'NONE', *, *, #17184, .T. ) ;
#7257 = CARTESIAN_POINT ( 'NONE',  ( 52.68750000000000711, 9.999999999999989342, 11.99999999999999467 ) ) ;
#7258 =( LENGTH_UNIT ( ) NAMED_UNIT ( * ) SI_UNIT ( .MILLI., .METRE. ) );
#7259 = CARTESIAN_POINT ( 'NONE',  ( 4.000000000000000000, 4.898587196589412829E-16, -2.074999997268812013 ) ) ;
#7260 = DIRECTION ( 'NONE',  ( 0.000000000000000000, 0.000000000000000000, 1.000000000000000000 ) ) ;
#7261 = ORIENTED_EDGE ( 'NONE', *, *, #17014, .T. ) ;
#7262 = VERTEX_POINT ( 'NONE', #2980 ) ;
#7263 = CARTESIAN_POINT ( 'NONE',  ( -1.656854249492380138, -3.999999999999999112, 18.18750000000001066 ) ) ;
#7264 = ORIENTED_EDGE ( 'NONE', *, *, #7667, .T. ) ;
#7265 = VECTOR ( 'NONE', #1660, 1000.000000000000000 ) ;
#7266 = DIRECTION ( 'NONE',  ( 0.000000000000000000, 0.000000000000000000, 1.000000000000000000 ) ) ;
#7267 = CARTESIAN_POINT ( 'NONE',  ( 4.999999999999999112, 6.807171995660675101, -6.478011392632816445 ) ) ;
#7268 = ORIENTED_EDGE ( 'NONE', *, *, #16511, .F. ) ;
#7269 = CARTESIAN_POINT ( 'NONE',  ( 35.00000000000000000, 4.500000000000001776, -20.00000000000000355 ) ) ;
#7270 = CARTESIAN_POINT ( 'NONE',  ( 45.00000000000000000, -9.796556200126357083, 11.00000000000008882 ) ) ;
#7271 = VECTOR ( 'NONE', #20339, 1000.000000000000000 ) ;
#7272 = CARTESIAN_POINT ( 'NONE',  ( 1.432654583217640276, 3.458734125000000770, 1.675000001365597235 ) ) ;
#7273 = CIRCLE ( 'NONE', #20625, 5.000000000000011546 ) ;
#7274 = CARTESIAN_POINT ( 'NONE',  ( 70.20000000000000284, 8.232233047033627571, 16.76776695296636532 ) ) ;
#7275 = PRODUCT_DEFINITION ( 'UNKNOWN', '', #6873, #22705 ) ;
#7276 = DIRECTION ( 'NONE',  ( -1.000000000000000000, -0.000000000000000000, -0.000000000000000000 ) ) ;
#7277 = ADVANCED_FACE ( 'NONE', ( #7679 ), #1454, .F. ) ;
#7278 = DIRECTION ( 'NONE',  ( 0.000000000000000000, 0.000000000000000000, 1.000000000000000000 ) ) ;
#7279 =( GEOMETRIC_REPRESENTATION_CONTEXT ( 3 ) GLOBAL_UNCERTAINTY_ASSIGNED_CONTEXT ( ( #19577 ) ) GLOBAL_UNIT_ASSIGNED_CONTEXT ( ( #22806, #8223, #1234 ) ) REPRESENTATION_CONTEXT ( 'NONE', 'WORKASPACE' ) );
#7280 = CARTESIAN_POINT ( 'NONE',  ( 53.18981816583844591, 9.931948859054346102, 10.99999999999999467 ) ) ;
#7281 = CARTESIAN_POINT ( 'NONE',  ( -2.117863837641485618E-16, 3.458734125000000326, -1.512499998634402987 ) ) ;
#7282 = CYLINDRICAL_SURFACE ( 'NONE', #18714, 2.500000000000002220 ) ;
#7283 = CARTESIAN_POINT ( 'NONE',  ( 4.000000000000000888, 4.898587196589412829E-16, 18.62500000273119483 ) ) ;
#7284 = CARTESIAN_POINT ( 'NONE',  ( 35.00000000000000000, 4.500000000000009770, -4.286263797015736496E-15 ) ) ;
#7285 = ORIENTED_EDGE ( 'NONE', *, *, #11592, .T. ) ;
#7286 = CARTESIAN_POINT ( 'NONE',  ( 4.000000000000000888, 1.656854249492381248, 11.68750000273119660 ) ) ;
#7287 =( BOUNDED_SURFACE ( )  B_SPLINE_SURFACE ( 3, 2, ( 
 ( #17676, #19680, #10396 ),
 ( #1239, #10627, #17903 ),
 ( #1480, #8822, #23403 ),
 ( #7009, #14326, #5200 ),
 ( #16938, #1951, #18602 ),
 ( #14929, #16823, #2315 ) ),
 .UNSPECIFIED., .F., .F., .F. ) 
 B_SPLINE_SURFACE_WITH_KNOTS ( ( 4, 2, 4 ),
 ( 3, 3 ),
 ( 0.02032853247518126918, 0.02278863295364821906, 0.02524873343211516893 ),
 ( 0.000000000000000000, 1.000000000000000000 ),
 .UNSPECIFIED. ) 
 GEOMETRIC_REPRESENTATION_ITEM ( )  RATIONAL_B_SPLINE_SURFACE ( (
 ( 1.000000000000000000, 0.8047781615896838492, 1.000000000000000000),
 ( 1.000000000000000000, 0.8123767586288186404, 1.000000000000000000),
 ( 1.000000000000000000, 0.8190662415565814758, 1.000000000000000000),
 ( 1.000000000000000000, 0.8192361015667604107, 1.000000000000000000),
 ( 1.000000000000000000, 0.8126135807104967190, 1.000000000000000000),
 ( 1.000000000000000000, 0.8047712338318580017, 1.000000000000000000) ) ) 
 REPRESENTATION_ITEM ( '' )  SURFACE ( )  );
#7288 = CARTESIAN_POINT ( 'NONE',  ( 32.96263968033274949, -11.25000000000000355, 10.00000000000008882 ) ) ;
#7289 = DIRECTION ( 'NONE',  ( -0.000000000000000000, -0.000000000000000000, -1.000000000000000000 ) ) ;
#7290 = ORIENTED_EDGE ( 'NONE', *, *, #21930, .T. ) ;
#7291 = CIRCLE ( 'NONE', #13363, 2.100000000000000089 ) ;
#7292 = VERTEX_POINT ( 'NONE', #10608 ) ;
#7293 = AXIS2_PLACEMENT_3D ( 'NONE', #5406, #122, #16660 ) ;
#7294 = LINE ( 'NONE', #8857, #16024 ) ;
#7295 = EDGE_LOOP ( 'NONE', ( #19397, #22480, #20882, #5603, #17634 ) ) ;
#7296 = CARTESIAN_POINT ( 'NONE',  ( 57.00000000000000000, 12.82842712474617741, 12.17157287525379239 ) ) ;
#7297 = ORIENTED_EDGE ( 'NONE', *, *, #1901, .F. ) ;
#7298 = CARTESIAN_POINT ( 'NONE',  ( -19.99999999999999645, -9.000000000000003553, 5.000000000000079936 ) ) ;
#7299 = ORIENTED_EDGE ( 'NONE', *, *, #1992, .F. ) ;
#7300 = VECTOR ( 'NONE', #18307, 1000.000000000000000 ) ;
#7301 = CARTESIAN_POINT ( 'NONE',  ( 55.06481816583844591, 5.999999999999996447, 15.06805114094564502 ) ) ;
#7302 = CIRCLE ( 'NONE', #9221, 4.000000000000001776 ) ;
#7303 = CARTESIAN_POINT ( 'NONE',  ( 69.30000000218494449, 11.76776695296636888, 16.76776695296636532 ) ) ;
#7304 = DIRECTION ( 'NONE',  ( 7.087422195345010423E-32, 0.9396926207859083169, 0.3420201433256690460 ) ) ;
#7305 = DIRECTION ( 'NONE',  ( -1.000000000000000000, -0.000000000000000000, -0.000000000000000000 ) ) ;
#7306 = DIRECTION ( 'NONE',  ( -0.9396926207859107594, -0.3420201433256623291, 1.540743955509804830E-32 ) ) ;
#7307 = VERTEX_POINT ( 'NONE', #11388 ) ;
#7308 = CARTESIAN_POINT ( 'NONE',  ( 2.828427124746192067, -2.828427124746189847, 16.50000000273119838 ) ) ;
#7309 = EDGE_CURVE ( 'NONE', #14277, #9347, #15629, .T. ) ;
#7310 = CARTESIAN_POINT ( 'NONE',  ( -2.828427124746189403, 2.828427124746190291, 10.00000000273119660 ) ) ;
#7311 = ADVANCED_FACE ( 'NONE', ( #17880 ), #8148, .T. ) ;
#7312 = CARTESIAN_POINT ( 'NONE',  ( 52.84143183416158251, 8.689308171935088865, 17.97181229448535689 ) ) ;
#7313 = LINE ( 'NONE', #327, #19538 ) ;
#7314 = CARTESIAN_POINT ( 'NONE',  ( 4.999999999999999112, 4.057423117305515525, -8.475820894092930047 ) ) ;
#7315 = AXIS2_PLACEMENT_3D ( 'NONE', #7685, #15003, #13193 ) ;
#7316 = CARTESIAN_POINT ( 'NONE',  ( -67.89999999999999147, 7.499999999999996447, 14.99999999999999645 ) ) ;
#7317 = DIRECTION ( 'NONE',  ( 1.000000000000000000, 0.000000000000000000, -1.224646799147353207E-16 ) ) ;
#7318 = AXIS2_PLACEMENT_3D ( 'NONE', #3111, #10686, #17843 ) ;
#7319 = ORIENTED_EDGE ( 'NONE', *, *, #27, .F. ) ;
#7320 = CARTESIAN_POINT ( 'NONE',  ( 4.000000000000000000, 2.309401076758497151, -5.000000000000000000 ) ) ;
#7321 = CARTESIAN_POINT ( 'NONE',  ( 56.43750000000000000, 10.00000000000000711, 17.99999999999999645 ) ) ;
#7322 = DIRECTION ( 'NONE',  ( 0.000000000000000000, 0.000000000000000000, 1.000000000000000000 ) ) ;
#7323 = EDGE_CURVE ( 'NONE', #18054, #14420, #17118, .T. ) ;
#7324 = ORIENTED_EDGE ( 'NONE', *, *, #11048, .F. ) ;
#7325 = DIRECTION ( 'NONE',  ( 0.3420201433256622181, 0.9396926207859107594, -6.162975822039141593E-32 ) ) ;
#7326 = LINE ( 'NONE', #13299, #5632 ) ;
#7327 = VERTEX_POINT ( 'NONE', #20806 ) ;
#7328 = CARTESIAN_POINT ( 'NONE',  ( -27.50000000000000711, 4.500000000000001776, -31.01025403784447221 ) ) ;
#7329 = ORIENTED_EDGE ( 'NONE', *, *, #2258, .T. ) ;
#7330 =( BOUNDED_CURVE ( )  B_SPLINE_CURVE ( 2, ( #13232, #10961, #20498 ),
 .UNSPECIFIED., .F., .F. ) 
 B_SPLINE_CURVE_WITH_KNOTS ( ( 3, 3 ),
 ( 0.9235200992307018852, 0.9250000000000000444 ),
 .UNSPECIFIED. ) 
 CURVE ( )  GEOMETRIC_REPRESENTATION_ITEM ( )  RATIONAL_B_SPLINE_CURVE ( ( 0.9841097943611589738, 0.9909879409283294249, 1.000000000000000000 ) ) 
 REPRESENTATION_ITEM ( '' )  );
#7331 = FACE_OUTER_BOUND ( 'NONE', #23174, .T. ) ;
#7332 = CARTESIAN_POINT ( 'NONE',  ( 4.000000000000001776, -1.656854249492379694, 17.43750000000001421 ) ) ;
#7333 = CARTESIAN_POINT ( 'NONE',  ( -4.000000000000000888, 1.563622288139195238, -0.2253451193528307472 ) ) ;
#7334 = AXIS2_PLACEMENT_3D ( 'NONE', #17375, #12002, #21168 ) ;
#7335 = APPLICATION_CONTEXT ( 'automotive_design' ) ;
#7336 = CARTESIAN_POINT ( 'NONE',  ( -3.999999999999999112, 1.656854249492380582, 10.93750000000001243 ) ) ;
#7337 = EDGE_CURVE ( 'NONE', #10020, #6374, #22614, .T. ) ;
#7338 = SURFACE_STYLE_USAGE ( .BOTH. , #8769 ) ;
#7339 = LINE ( 'NONE', #23365, #9080 ) ;
#7340 = CARTESIAN_POINT ( 'NONE',  ( -68.05000000000002558, 8.964466094067258695, 12.49999999999999289 ) ) ;
#7341 = EDGE_CURVE ( 'NONE', #20172, #13175, #11425, .T. ) ;
#7342 = CARTESIAN_POINT ( 'NONE',  ( -1.656854249492381248, -3.999999999999999112, -0.3874999972688122907 ) ) ;
#7343 = CARTESIAN_POINT ( 'NONE',  ( -3.458734124999998993, 1.432654583217640276, 19.37500000136560274 ) ) ;
#7344 = CYLINDRICAL_SURFACE ( 'NONE', #7293, 8.749000000000002331 ) ;
#7345 = CARTESIAN_POINT ( 'NONE',  ( 7.347880794884118750E-16, -4.000000000000000000, 3.550000000000002931 ) ) ;
#7346 = CARTESIAN_POINT ( 'NONE',  ( 67.74999999999997158, 8.964466094067246260, 17.49999999999999289 ) ) ;
#7347 = CARTESIAN_POINT ( 'NONE',  ( -3.458734124999998993, 1.432654583217640276, 14.37500000136560452 ) ) ;
#7348 = CYLINDRICAL_SURFACE ( 'NONE', #14949, 2.500000000000002220 ) ;
#7349 = ADVANCED_FACE ( 'NONE', ( #2377 ), #4176, .T. ) ;
#7350 = EDGE_CURVE ( 'NONE', #1924, #2020, #12575, .T. ) ;
#7351 = ORIENTED_EDGE ( 'NONE', *, *, #12425, .T. ) ;
#7352 = CARTESIAN_POINT ( 'NONE',  ( -68.70000000109247651, 12.06698729999999919, 15.85617417291294196 ) ) ;
#7353 = EDGE_LOOP ( 'NONE', ( #21057, #14903 ) ) ;
#7354 = CARTESIAN_POINT ( 'NONE',  ( 54.99768183416157541, 12.87654654797631792, 12.21969229848393113 ) ) ;
#7355 = CARTESIAN_POINT ( 'NONE',  ( -71.30000000109247082, 12.06698730000000275, 15.85617417291294196 ) ) ;
#7356 = DIRECTION ( 'NONE',  ( -1.000000000000000000, -2.217193442732859957E-17, 5.551115123125786400E-17 ) ) ;
#7357 = CARTESIAN_POINT ( 'NONE',  ( 19.56809120928344825, -8.974600000000002353, 5.000000000000079936 ) ) ;
#7358 = ORIENTED_EDGE ( 'NONE', *, *, #5696, .T. ) ;
#7359 = ORIENTED_EDGE ( 'NONE', *, *, #8838, .F. ) ;
#7360 = CARTESIAN_POINT ( 'NONE',  ( -1.489200000000000079, 0.000000000000000000, 0.000000000000000000 ) ) ;
#7361 = CARTESIAN_POINT ( 'NONE',  ( 53.65856816583844591, 7.028187705514647554, 16.31069182806492179 ) ) ;
#7362 = CARTESIAN_POINT ( 'NONE',  ( -70.15000000109247935, 11.46158073645647235, 13.53841926354352232 ) ) ;
#7363 = CARTESIAN_POINT ( 'NONE',  ( -69.50000000109247367, 10.85617417291294551, 12.93301269999999370 ) ) ;
#7364 = CARTESIAN_POINT ( 'NONE',  ( -1.432654583217639166, 3.458734125000000770, 13.50000000136560452 ) ) ;
#7365 = EDGE_CURVE ( 'NONE', #14744, #5198, #9707, .T. ) ;
#7366 = DIRECTION ( 'NONE',  ( 0.000000000000000000, 1.000000000000000000, -0.000000000000000000 ) ) ;
#7367 = CARTESIAN_POINT ( 'NONE',  ( 55.40625000000000000, 12.99999999999999645, 13.75735931288070191 ) ) ;
#7368 = CARTESIAN_POINT ( 'NONE',  ( 65.00000000000000000, 9.999999999999998224, 14.99999999999999645 ) ) ;
#7369 = ADVANCED_FACE ( 'NONE', ( #15220 ), #21039, .F. ) ;
#7370 = CARTESIAN_POINT ( 'NONE',  ( 56.25000000000000711, 7.878679656440361612, 17.12132034355964549 ) ) ;
#7371 = CARTESIAN_POINT ( 'NONE',  ( 4.000000000000000888, 4.898587196589412829E-16, 17.62500000273119483 ) ) ;
#7372 = ADVANCED_FACE ( 'NONE', ( #2728 ), #18902, .T. ) ;
#7373 = CARTESIAN_POINT ( 'NONE',  ( 60.00000000000000000, -10.00000000000000178, 12.49999999999999467 ) ) ;
#7374 = ADVANCED_FACE ( 'NONE', ( #15346 ), #22485, .T. ) ;
#7375 = ORIENTED_EDGE ( 'NONE', *, *, #20158, .F. ) ;
#7376 = DIRECTION ( 'NONE',  ( 0.000000000000000000, 0.000000000000000000, -1.000000000000000000 ) ) ;
#7377 = LINE ( 'NONE', #11450, #4390 ) ;
#7378 = EDGE_LOOP ( 'NONE', ( #18737, #22846, #14367, #11154 ) ) ;
#7379 = CARTESIAN_POINT ( 'NONE',  ( 57.00000000000000000, 12.12132034355963484, 12.87867965644034740 ) ) ;
#7380 =( LENGTH_UNIT ( ) NAMED_UNIT ( * ) SI_UNIT ( .MILLI., .METRE. ) );
#7381 = CARTESIAN_POINT ( 'NONE',  ( -3.458734125000000326, 1.432654583217640276, 5.675000001365596347 ) ) ;
#7382 = LINE ( 'NONE', #13247, #590 ) ;
#7383 = ORIENTED_EDGE ( 'NONE', *, *, #18009, .F. ) ;
#7384 = CARTESIAN_POINT ( 'NONE',  ( 9.920644283265380691E-16, 4.000000000000000000, 15.75000000000001066 ) ) ;
#7385 = DIRECTION ( 'NONE',  ( 0.000000000000000000, 0.000000000000000000, 1.000000000000000000 ) ) ;
#7386 = CARTESIAN_POINT ( 'NONE',  ( -54.99999999999992895, -15.00000000000000000, 1.387778780781445676E-14 ) ) ;
#7387 = VERTEX_POINT ( 'NONE', #20916 ) ;
#7388 = CARTESIAN_POINT ( 'NONE',  ( -27.50000000000000711, 7.500000000000002665, -36.31025403784445160 ) ) ;
#7389 = DIRECTION ( 'NONE',  ( 1.000000000000000000, 7.703719777548943412E-32, 0.000000000000000000 ) ) ;
#7390 = CARTESIAN_POINT ( 'NONE',  ( -3.458734125000000326, -1.432654583217642497, -0.9499999986344030978 ) ) ;
#7391 = CARTESIAN_POINT ( 'NONE',  ( 68.25000000000000000, 12.50000000000000000, 13.96446609406725869 ) ) ;
#7392 = CARTESIAN_POINT ( 'NONE',  ( 0.000000000000000000, 0.000000000000000000, 0.000000000000000000 ) ) ;
#7393 = PLANE ( 'NONE',  #14942 ) ;
#7394 = CARTESIAN_POINT ( 'NONE',  ( 53.09606816583843170, 11.58880310854672935, 10.97181229448534445 ) ) ;
#7395 = CARTESIAN_POINT ( 'NONE',  ( -3.458734125000000326, 1.432654583217640276, -0.3249999986344045411 ) ) ;
#7396 = CARTESIAN_POINT ( 'NONE',  ( -3.458734124999998993, 1.432654583217640276, 10.37500000136560629 ) ) ;
#7397 = EDGE_CURVE ( 'NONE', #12358, #8470, #21301, .T. ) ;
#7398 = LINE ( 'NONE', #3654, #19089 ) ;
#7399 = DIRECTION ( 'NONE',  ( 1.000000000000000000, 0.000000000000000000, -0.000000000000000000 ) ) ;
#7400 = CARTESIAN_POINT ( 'NONE',  ( -35.00000000000000000, 7.500000000000001776, -19.99999999999998934 ) ) ;
#7401 = ORIENTED_EDGE ( 'NONE', *, *, #22798, .F. ) ;
#7402 = CARTESIAN_POINT ( 'NONE',  ( 18.97172504071656363, -8.974600000000002353, 5.000000000000079936 ) ) ;
#7403 = CYLINDRICAL_SURFACE ( 'NONE', #1842, 11.00000000000000000 ) ;
#7404 = CYLINDRICAL_SURFACE ( 'NONE', #9763, 2.500000000000002220 ) ;
#7405 = ORIENTED_EDGE ( 'NONE', *, *, #6198, .F. ) ;
#7406 = ORIENTED_EDGE ( 'NONE', *, *, #14371, .T. ) ;
#7407 = LINE ( 'NONE', #11237, #7188 ) ;
#7408 = ORIENTED_EDGE ( 'NONE', *, *, #3373, .T. ) ;
#7409 = CARTESIAN_POINT ( 'NONE',  ( 54.93750000000000711, 10.00000000000001776, 18.99999999999999645 ) ) ;
#7410 = VERTEX_POINT ( 'NONE', #8262 ) ;
#7411 = CARTESIAN_POINT ( 'NONE',  ( 4.000000000000000888, 4.898587196589412829E-16, 13.62500000273119660 ) ) ;
#7412 = ORIENTED_EDGE ( 'NONE', *, *, #15246, .T. ) ;
#7413 = AXIS2_PLACEMENT_3D ( 'NONE', #3576, #14386, #22114 ) ;
#7414 = CARTESIAN_POINT ( 'NONE',  ( 57.03356816583845301, 11.72490539043803004, 18.97181229448534268 ) ) ;
#7415 = CARTESIAN_POINT ( 'NONE',  ( 71.80000000109247082, 12.06698730000000275, 14.14382582708705094 ) ) ;
#7416 = DIRECTION ( 'NONE',  ( 0.000000000000000000, 0.9510565162951521989, 0.3090169943749515591 ) ) ;
#7417 = CARTESIAN_POINT ( 'NONE',  ( 71.25000000109247367, 12.06698730000000097, 14.99999999999999645 ) ) ;
#7418 = CARTESIAN_POINT ( 'NONE',  ( 118.3095189484530181, -7.098169556225942145, 56.71010071662853136 ) ) ;
#7419 = VERTEX_POINT ( 'NONE', #13429 ) ;
#7420 = CARTESIAN_POINT ( 'NONE',  ( -3.999999999999999112, 1.656854249492380804, 17.06250000273120193 ) ) ;
#7421 = CARTESIAN_POINT ( 'NONE',  ( -2.805705207896067144, 3.226868319750155312, -3.503898532754364581 ) ) ;
#7422 =( BOUNDED_SURFACE ( )  B_SPLINE_SURFACE ( 1, 2, ( 
 ( #5601, #5721, #11138, #12927, #20189, #15088, #9330, #4036, #5957, #14975, #3911, #4156, #16981, #16740, #320, #2355, #18412, #2234, #17094, #555, #7417, #2466, #22343, #4279, #11613, #3799, #13407, #20426, #444, #16622, #200, #7531, #14847, #22101, #13053, #11247, #18523, #2108, #9576, #11503, #9445, #5837, #11369, #7769, #18774, #9686, #7880, #15198, #18881, #9803, #22707, #18994, #10411, #10051, #21133, #668, #10287, #6436, #9927, #6319, #8004, #15441, #15789, #2823, #21247, #13875, #8243, #17339, #21018, #17226, #6672, #799, #13755, #1144, #6201, #23060, #907, #11845, #10170, #19123, #22596, #15562, #1025, #19347, #4865, #19470, #13634, #17462, #13985, #4633, #20785, #8130, #13519, #4747, #12200, #20895, #3068, #15327, #8486, #4391, #11730, #2583, #4510, #8359, #2710, #22822, #11968, #19233, #12080, #15676, #22952, #2937, #6559, #17576, #8710, #4992, #15898, #16014, #21370, #23176, #8591, #1616, #19582, #14344, #16248, #17918, #6913, #14463, #3539 ),
 ( #12559, #3646, #10874, #17691, #12791, #8958, #14590, #21849, #14107, #16364, #23420, #3425, #1253, #6785, #17801, #12320, #1372, #3179, #21486, #10525, #5099, #19820, #23539, #23304, #14230, #21607, #12433, #19697, #3300, #10644, #1501, #8843, #16138, #7149, #18148, #7028, #5215, #10765, #18041, #21728, #5341, #1732, #12684, #19937, #9072, #23659, #7274, #5454, #20043, #7744, #10983, #20520, #16711, #20159, #9304, #18262, #1964, #2330, #13137, #7852, #417, #18496, #20285, #7621, #3764, #16953, #11105, #289, #11469, #16481, #9663, #3886, #22070, #20400, #5687, #9196, #2079, #11346, #5929, #15177, #6049, #16595, #4007, #531, #14944, #7391, #18385, #59, #15059, #22435, #170, #13377, #20648, #18746, #1846, #14701, #21957, #5571, #18615, #12898, #7505, #14819, #13024, #22316, #11220, #2205, #13259, #9420, #22198, #5810, #9543, #16838, #4127, #7978, #2440, #18854, #11944, #6176, #881, #2797, #4478, #17194, #997, #13850, #13606, #20870, #22919, #15296, #22797 ) ),
 .UNSPECIFIED., .F., .F., .F. ) 
 B_SPLINE_SURFACE_WITH_KNOTS ( ( 2, 2 ),
 ( 3, 2, 2, 2, 2, 2, 2, 2, 2, 2, 2, 2, 2, 2, 2, 2, 2, 2, 2, 2, 2, 2, 2, 2, 2, 2, 2, 2, 2, 2, 2, 2, 2, 2, 2, 2, 2, 2, 2, 2, 2, 2, 2, 2, 2, 2, 2, 2, 2, 2, 2, 2, 2, 2, 2, 2, 2, 2, 2, 2, 2, 2, 2, 2, 3 ),
 ( 0.000000000000000000, 1.000000000000000000 ),
 ( 0.000000000000000000, 0.01562500000000000000, 0.03125000000000000000, 0.04687500000000000000, 0.06250000000000000000, 0.07812500000000000000, 0.09375000000000000000, 0.1093750000000000000, 0.1250000000000000000, 0.1406250000000000000, 0.1562500000000000000, 0.1718750000000000000, 0.1875000000000000000, 0.2031250000000000000, 0.2187500000000000000, 0.2343750000000000000, 0.2500000000000000000, 0.2656250000000000000, 0.2812500000000000000, 0.2968750000000000000, 0.3125000000000000000, 0.3281250000000000000, 0.3437500000000000000, 0.3593750000000000000, 0.3750000000000000000, 0.3906250000000000000, 0.4062500000000000000, 0.4218750000000000000, 0.4375000000000000000, 0.4531250000000000000, 0.4687500000000000000, 0.4843750000000000000, 0.5000000000000000000, 0.5156250000000000000, 0.5312500000000000000, 0.5468750000000000000, 0.5625000000000000000, 0.5781250000000000000, 0.5937500000000000000, 0.6093750000000000000, 0.6250000000000000000, 0.6406250000000000000, 0.6562500000000000000, 0.6718750000000000000, 0.6875000000000000000, 0.7031250000000000000, 0.7187500000000000000, 0.7343750000000000000, 0.7500000000000000000, 0.7656250000000000000, 0.7812500000000000000, 0.7968750000000000000, 0.8125000000000000000, 0.8281250000000000000, 0.8437500000000000000, 0.8593750000000000000, 0.8750000000000000000, 0.8906250000000000000, 0.9062500000000000000, 0.9218750000000000000, 0.9375000000000000000, 0.9531250000000000000, 0.9687500000000000000, 0.9843750000000000000, 1.000000000000000000 ),
 .UNSPECIFIED. ) 
 GEOMETRIC_REPRESENTATION_ITEM ( )  RATIONAL_B_SPLINE_SURFACE ( (
 ( 1.000000000000000000, 0.9238795325112867385, 1.000000000000000000, 0.9238795325112867385, 1.000000000000000000, 0.9238795325112867385, 1.000000000000000000, 0.9238795325112867385, 1.000000000000000000, 0.9238795325112867385, 1.000000000000000000, 0.9238795325112867385, 1.000000000000000000, 0.9238795325112867385, 1.000000000000000000, 0.9238795325112867385, 1.000000000000000000, 0.9238795325112867385, 1.000000000000000000, 0.9238795325112867385, 1.000000000000000000, 0.9238795325112867385, 1.000000000000000000, 0.9238795325112867385, 1.000000000000000000, 0.9238795325112867385, 1.000000000000000000, 0.9238795325112867385, 1.000000000000000000, 0.9238795325112867385, 1.000000000000000000, 0.9238795325112867385, 1.000000000000000000, 0.9238795325112867385, 1.000000000000000000, 0.9238795325112867385, 1.000000000000000000, 0.9238795325112867385, 1.000000000000000000, 0.9238795325112867385, 1.000000000000000000, 0.9238795325112867385, 1.000000000000000000, 0.9238795325112867385, 1.000000000000000000, 0.9238795325112867385, 1.000000000000000000, 0.9238795325112867385, 1.000000000000000000, 0.9238795325112867385, 1.000000000000000000, 0.9238795325112867385, 1.000000000000000000, 0.9238795325112867385, 1.000000000000000000, 0.9238795325112867385, 1.000000000000000000, 0.9238795325112867385, 1.000000000000000000, 0.9238795325112867385, 1.000000000000000000, 0.9238795325112867385, 1.000000000000000000, 0.9238795325112867385, 1.000000000000000000, 0.9238795325112867385, 1.000000000000000000, 0.9238795325112867385, 1.000000000000000000, 0.9238795325112867385, 1.000000000000000000, 0.9238795325112867385, 1.000000000000000000, 0.9238795325112867385, 1.000000000000000000, 0.9238795325112867385, 1.000000000000000000, 0.9238795325112867385, 1.000000000000000000, 0.9238795325112867385, 1.000000000000000000, 0.9238795325112867385, 1.000000000000000000, 0.9238795325112867385, 1.000000000000000000, 0.9238795325112867385, 1.000000000000000000, 0.9238795325112867385, 1.000000000000000000, 0.9238795325112867385, 1.000000000000000000, 0.9238795325112867385, 1.000000000000000000, 0.9238795325112867385, 1.000000000000000000, 0.9238795325112867385, 1.000000000000000000, 0.9238795325112867385, 1.000000000000000000, 0.9238795325112867385, 1.000000000000000000, 0.9238795325112867385, 1.000000000000000000, 0.9238795325112867385, 1.000000000000000000, 0.9238795325112867385, 1.000000000000000000, 0.9238795325112867385, 1.000000000000000000, 0.9238795325112867385, 1.000000000000000000, 0.9238795325112867385, 1.000000000000000000, 0.9238795325112867385, 1.000000000000000000, 0.9238795325112867385, 1.000000000000000000, 0.9238795325112867385, 1.000000000000000000, 0.9238795325112867385, 1.000000000000000000, 0.9238795325112867385, 1.000000000000000000, 0.9238795325112867385, 1.000000000000000000, 0.9238795325112867385, 1.000000000000000000, 0.9238795325112867385, 1.000000000000000000),
 ( 1.000000000000000000, 0.9238795325112867385, 1.000000000000000000, 0.9238795325112867385, 1.000000000000000000, 0.9238795325112867385, 1.000000000000000000, 0.9238795325112867385, 1.000000000000000000, 0.9238795325112867385, 1.000000000000000000, 0.9238795325112867385, 1.000000000000000000, 0.9238795325112867385, 1.000000000000000000, 0.9238795325112867385, 1.000000000000000000, 0.9238795325112867385, 1.000000000000000000, 0.9238795325112867385, 1.000000000000000000, 0.9238795325112867385, 1.000000000000000000, 0.9238795325112867385, 1.000000000000000000, 0.9238795325112867385, 1.000000000000000000, 0.9238795325112867385, 1.000000000000000000, 0.9238795325112867385, 1.000000000000000000, 0.9238795325112867385, 1.000000000000000000, 0.9238795325112867385, 1.000000000000000000, 0.9238795325112867385, 1.000000000000000000, 0.9238795325112867385, 1.000000000000000000, 0.9238795325112867385, 1.000000000000000000, 0.9238795325112867385, 1.000000000000000000, 0.9238795325112867385, 1.000000000000000000, 0.9238795325112867385, 1.000000000000000000, 0.9238795325112867385, 1.000000000000000000, 0.9238795325112867385, 1.000000000000000000, 0.9238795325112867385, 1.000000000000000000, 0.9238795325112867385, 1.000000000000000000, 0.9238795325112867385, 1.000000000000000000, 0.9238795325112867385, 1.000000000000000000, 0.9238795325112867385, 1.000000000000000000, 0.9238795325112867385, 1.000000000000000000, 0.9238795325112867385, 1.000000000000000000, 0.9238795325112867385, 1.000000000000000000, 0.9238795325112867385, 1.000000000000000000, 0.9238795325112867385, 1.000000000000000000, 0.9238795325112867385, 1.000000000000000000, 0.9238795325112867385, 1.000000000000000000, 0.9238795325112867385, 1.000000000000000000, 0.9238795325112867385, 1.000000000000000000, 0.9238795325112867385, 1.000000000000000000, 0.9238795325112867385, 1.000000000000000000, 0.9238795325112867385, 1.000000000000000000, 0.9238795325112867385, 1.000000000000000000, 0.9238795325112867385, 1.000000000000000000, 0.9238795325112867385, 1.000000000000000000, 0.9238795325112867385, 1.000000000000000000, 0.9238795325112867385, 1.000000000000000000, 0.9238795325112867385, 1.000000000000000000, 0.9238795325112867385, 1.000000000000000000, 0.9238795325112867385, 1.000000000000000000, 0.9238795325112867385, 1.000000000000000000, 0.9238795325112867385, 1.000000000000000000, 0.9238795325112867385, 1.000000000000000000, 0.9238795325112867385, 1.000000000000000000, 0.9238795325112867385, 1.000000000000000000, 0.9238795325112867385, 1.000000000000000000, 0.9238795325112867385, 1.000000000000000000, 0.9238795325112867385, 1.000000000000000000, 0.9238795325112867385, 1.000000000000000000, 0.9238795325112867385, 1.000000000000000000, 0.9238795325112867385, 1.000000000000000000, 0.9238795325112867385, 1.000000000000000000, 0.9238795325112867385, 1.000000000000000000, 0.9238795325112867385, 1.000000000000000000) ) ) 
 REPRESENTATION_ITEM ( '' )  SURFACE ( )  );
#7423 = CARTESIAN_POINT ( 'NONE',  ( 59.34375000000000711, 8.343145750507638070, 19.00000000000000711 ) ) ;
#7424 = CARTESIAN_POINT ( 'NONE',  ( 2.974182810908596597, -5.788408252967910173, -3.700000000000000178 ) ) ;
#7425 = CARTESIAN_POINT ( 'NONE',  ( 66.95000000218496439, 11.03553390593272887, 17.50000000000001066 ) ) ;
#7426 = CARTESIAN_POINT ( 'NONE',  ( -69.09999999999999432, 12.50000000000000000, 14.99999999999999645 ) ) ;
#7427 = AXIS2_PLACEMENT_3D ( 'NONE', #7392, #7507, #5342 ) ;
#7428 = CARTESIAN_POINT ( 'NONE',  ( 3.999999999999998224, 2.472263674411418588, -3.687027874309861897 ) ) ;
#7429 = VERTEX_POINT ( 'NONE', #17359 ) ;
#7430 = DIRECTION ( 'NONE',  ( -1.000000000000000000, 0.000000000000000000, 0.000000000000000000 ) ) ;
#7431 = CARTESIAN_POINT ( 'NONE',  ( 4.999999999999999112, -8.475820894093002877, 4.057423117305363647 ) ) ;
#7432 = ORIENTED_EDGE ( 'NONE', *, *, #8689, .T. ) ;
#7433 = DIRECTION ( 'NONE',  ( 0.3420201433256622736, -0.9396926207859106484, -1.232595164407828100E-31 ) ) ;
#7434 = LINE ( 'NONE', #14747, #14058 ) ;
#7435 = CARTESIAN_POINT ( 'NONE',  ( 0.6448876103708359731, 4.246476118072354922, -0.2256878752776725616 ) ) ;
#7436 = EDGE_LOOP ( 'NONE', ( #13337, #14281, #4682, #12013 ) ) ;
#7437 = LINE ( 'NONE', #21783, #6836 ) ;
#7438 = ORIENTED_EDGE ( 'NONE', *, *, #3345, .F. ) ;
#7439 = EDGE_CURVE ( 'NONE', #7929, #13418, #13869, .T. ) ;
#7440 = CARTESIAN_POINT ( 'NONE',  ( -3.999999999999999112, 0.000000000000000000, 15.12500000273119660 ) ) ;
#7441 = CARTESIAN_POINT ( 'NONE',  ( -2.828427124746189403, 2.828427124746190291, 19.87500000000001066 ) ) ;
#7442 = DIRECTION ( 'NONE',  ( -1.000000000000000000, -0.000000000000000000, -0.000000000000000000 ) ) ;
#7443 = CARTESIAN_POINT ( 'NONE',  ( -2.828427124746189403, 2.828427124746190291, 10.87500000000001066 ) ) ;
#7444 = DIRECTION ( 'NONE',  ( 0.000000000000000000, 0.000000000000000000, 1.000000000000000000 ) ) ;
#7445 = CARTESIAN_POINT ( 'NONE',  ( 0.000000000000000000, -2.223716399045629899, 8.461683424509306661 ) ) ;
#7446 = EDGE_CURVE ( 'NONE', #23552, #17274, #5726, .T. ) ;
#7447 = VERTEX_POINT ( 'NONE', #21629 ) ;
#7448 = CARTESIAN_POINT ( 'NONE',  ( -66.44999999999998863, 8.964466094067258695, 12.49999999999999289 ) ) ;
#7449 = CARTESIAN_POINT ( 'NONE',  ( 66.35000000218495586, 7.499999999999996447, 16.03553390593273775 ) ) ;
#7450 = CARTESIAN_POINT ( 'NONE',  ( 67.50000000109247367, 7.933012699999995476, 14.14382582708705094 ) ) ;
#7451 = CARTESIAN_POINT ( 'NONE',  ( -2.445694354108818303, -2.445694354108820523, 16.56250000136560629 ) ) ;
#7452 = DIRECTION ( 'NONE',  ( -1.000000000000000000, -0.000000000000000000, -0.000000000000000000 ) ) ;
#7453 = AXIS2_PLACEMENT_3D ( 'NONE', #19923, #3285, #21710 ) ;
#7454 = CARTESIAN_POINT ( 'NONE',  ( 2.828427124746190735, -2.828427124746189847, 5.675000000000001599 ) ) ;
#7455 = CARTESIAN_POINT ( 'NONE',  ( -1.656854249492379472, 4.000000000000000000, 12.81250000000001066 ) ) ;
#7456 = CARTESIAN_POINT ( 'NONE',  ( -1.432654583217639610, -3.458734124999999882, 12.62500000136560629 ) ) ;
#7457 = CARTESIAN_POINT ( 'NONE',  ( 4.999999999999999112, 9.314797388894893615, 1.239665997526919083 ) ) ;
#7458 = ORIENTED_EDGE ( 'NONE', *, *, #1427, .F. ) ;
#7459 = CARTESIAN_POINT ( 'NONE',  ( -67.60000000109248219, 9.143825827087052716, 12.93301269999999192 ) ) ;
#7460 = VERTEX_POINT ( 'NONE', #14125 ) ;
#7461 = CARTESIAN_POINT ( 'NONE',  ( 54.90393183416157541, 14.02818770551463956, 13.41119689145323335 ) ) ;
#7462 = CARTESIAN_POINT ( 'NONE',  ( -69.85000000109246798, 9.999999999999998224, 17.06698730000000097 ) ) ;
#7463 = CARTESIAN_POINT ( 'NONE',  ( 4.000000000000000888, 4.898587196589412829E-16, 21.31370849898476649 ) ) ;
#7464 = ORIENTED_EDGE ( 'NONE', *, *, #4965, .T. ) ;
#7465 = EDGE_CURVE ( 'NONE', #892, #16266, #11022, .T. ) ;
#7466 = EDGE_CURVE ( 'NONE', #3547, #12645, #12170, .T. ) ;
#7467 = VERTEX_POINT ( 'NONE', #1273 ) ;
#7468 = CARTESIAN_POINT ( 'NONE',  ( 3.458734125000001658, 4.235727675282972223E-16, 19.18750000136560629 ) ) ;
#7469 = CARTESIAN_POINT ( 'NONE',  ( 50.75231816583844591, 7.926799079670502124, 17.16943976678978245 ) ) ;
#7470 = AXIS2_PLACEMENT_3D ( 'NONE', #23318, #6926, #14243 ) ;
#7471 = VECTOR ( 'NONE', #4704, 1000.000000000000000 ) ;
#7472 = CARTESIAN_POINT ( 'NONE',  ( -65.70000000218495018, 8.232233047033629347, 13.23223304703362402 ) ) ;
#7473 = TOROIDAL_SURFACE ( 'NONE', #18155, 5.384454397937118664, 0.5155456020628804703 ) ;
#7474 = ADVANCED_FACE ( 'NONE', ( #12452 ), #1636, .T. ) ;
#7475 = ADVANCED_FACE ( 'NONE', ( #10429 ), #16363, .F. ) ;
#7476 = CARTESIAN_POINT ( 'NONE',  ( -68.75000000109245946, 11.46158073645647235, 13.53841926354352232 ) ) ;
#7477 = CARTESIAN_POINT ( 'NONE',  ( -2.445694354108818303, -2.445694354108820967, 12.81250000136560629 ) ) ;
#7478 = CARTESIAN_POINT ( 'NONE',  ( -4.197393957002303999, -7.773935952363655451E-14, -3.503767560748929810 ) ) ;
#7479 = CARTESIAN_POINT ( 'NONE',  ( 53.81250000000000711, 13.00000000000000000, 14.99999999999998757 ) ) ;
#7480 = CARTESIAN_POINT ( 'NONE',  ( 14.11308378033275446, -11.25000000000000355, 10.00000000000008882 ) ) ;
#7481 = CARTESIAN_POINT ( 'NONE',  ( 51.84375000000001421, 8.757359312880723223, 18.00000000000000355 ) ) ;
#7482 = CARTESIAN_POINT ( 'NONE',  ( -2.828427124746189403, 2.828427124746190291, 14.00000000273119660 ) ) ;
#7483 = CARTESIAN_POINT ( 'NONE',  ( 0.6666666666666689611, 4.233901974057261874, -3.300726591567082480 ) ) ;
#7484 = ORIENTED_EDGE ( 'NONE', *, *, #19484, .T. ) ;
#7485 = DIRECTION ( 'NONE',  ( -1.000000000000000000, 0.000000000000000000, 0.000000000000000000 ) ) ;
#7486 = CARTESIAN_POINT ( 'NONE',  ( -71.75000000218496155, 11.03553390593273953, 17.50000000000000355 ) ) ;
#7487 = ORIENTED_EDGE ( 'NONE', *, *, #5850, .F. ) ;
#7488 = CARTESIAN_POINT ( 'NONE',  ( 56.90625000000000711, 12.99999999999999645, 13.75735931288070191 ) ) ;
#7489 = AXIS2_PLACEMENT_3D ( 'NONE', #10454, #12010, #8527 ) ;
#7490 =( NAMED_UNIT ( * ) PLANE_ANGLE_UNIT ( ) SI_UNIT ( $, .RADIAN. ) );
#7491 = CARTESIAN_POINT ( 'NONE',  ( -2.828427124746189403, -2.828427124746190735, -3.449999997268813345 ) ) ;
#7492 = EDGE_CURVE ( 'NONE', #19414, #7327, #23230, .T. ) ;
#7493 = DIRECTION ( 'NONE',  ( -1.000000000000000000, 0.000000000000000000, 0.000000000000000000 ) ) ;
#7494 = ORIENTED_EDGE ( 'NONE', *, *, #18616, .T. ) ;
#7495 = CARTESIAN_POINT ( 'NONE',  ( 4.000000000000000888, 1.656854249492381248, 16.56250000000001066 ) ) ;
#7496 = CARTESIAN_POINT ( 'NONE',  ( 1.656854249492383024, -3.999999999999999112, -2.387499999999998401 ) ) ;
#7497 = ADVANCED_FACE ( 'NONE', ( #16035 ), #22971, .T. ) ;
#7498 = CARTESIAN_POINT ( 'NONE',  ( -0.7060087303327398089, -11.25000000000000355, 5.000000000000079936 ) ) ;
#7499 = ORIENTED_EDGE ( 'NONE', *, *, #1162, .F. ) ;
#7500 = CYLINDRICAL_SURFACE ( 'NONE', #17494, 9.999999999999996447 ) ;
#7501 = ADVANCED_FACE ( 'NONE', ( #6578 ), #9112, .T. ) ;
#7502 = CARTESIAN_POINT ( 'NONE',  ( -1.432654583217641164, -3.458734125000000326, 1.175000001365597013 ) ) ;
#7503 = EDGE_CURVE ( 'NONE', #23245, #9804, #10260, .T. ) ;
#7504 = AXIS2_PLACEMENT_3D ( 'NONE', #14662, #21919, #2043 ) ;
#7505 = CARTESIAN_POINT ( 'NONE',  ( 67.49999999999998579, 12.50000000000000000, 14.99999999999999645 ) ) ;
#7506 = CIRCLE ( 'NONE', #19326, 4.000000000000001776 ) ;
#7507 = DIRECTION ( 'NONE',  ( -1.000000000000000000, 0.000000000000000000, 0.000000000000000000 ) ) ;
#7508 = DIRECTION ( 'NONE',  ( 1.000000000000000000, 0.000000000000000000, 0.000000000000000000 ) ) ;
#7509 = CARTESIAN_POINT ( 'NONE',  ( 52.34606816583843880, 8.411196891453267099, 19.02818770551464667 ) ) ;
#7510 = CARTESIAN_POINT ( 'NONE',  ( 3.458734125000000326, 4.235727675282971730E-16, -0.7624999986344040970 ) ) ;
#7511 = CARTESIAN_POINT ( 'NONE',  ( -2.445694354108819191, 2.445694354108820523, 16.56250000136560629 ) ) ;
#7512 = LINE ( 'NONE', #2089, #14170 ) ;
#7513 = CARTESIAN_POINT ( 'NONE',  ( -71.85000000109246798, 9.999999999999998224, 12.93301269999999192 ) ) ;
#7514 = LINE ( 'NONE', #4138, #3279 ) ;
#7515 = ORIENTED_EDGE ( 'NONE', *, *, #3762, .F. ) ;
#7516 = DIRECTION ( 'NONE',  ( 1.000000000000000000, 0.000000000000000000, 0.000000000000000000 ) ) ;
#7517 = DIRECTION ( 'NONE',  ( -1.000000000000000000, 0.000000000000000000, 0.000000000000000000 ) ) ;
#7518 = DIRECTION ( 'NONE',  ( 0.3420201433256622736, 0.9396926207859106484, 0.000000000000000000 ) ) ;
#7519 = VERTEX_POINT ( 'NONE', #5233 ) ;
#7520 = VERTEX_POINT ( 'NONE', #6686 ) ;
#7521 = CARTESIAN_POINT ( 'NONE',  ( -20.00000000000001066, 4.500000000000001776, -49.99999999999999289 ) ) ;
#7522 = CARTESIAN_POINT ( 'NONE',  ( 57.37500000000000000, 7.171572875253794166, 12.17157287525381726 ) ) ;
#7523 = EDGE_LOOP ( 'NONE', ( #14303, #12118, #12803, #15708 ) ) ;
#7524 = DIRECTION ( 'NONE',  ( 1.000000000000000000, -0.000000000000000000, -0.000000000000000000 ) ) ;
#7525 = VERTEX_POINT ( 'NONE', #19720 ) ;
#7526 = CARTESIAN_POINT ( 'NONE',  ( 53.47106816583843880, 5.971812294485345340, 13.41119689145326710 ) ) ;
#7527 = EDGE_CURVE ( 'NONE', #8578, #10489, #12100, .T. ) ;
#7528 = CARTESIAN_POINT ( 'NONE',  ( 70.45000000109247651, 9.999999999999998224, 17.06698730000000097 ) ) ;
#7529 = EDGE_CURVE ( 'NONE', #17653, #18371, #15807, .T. ) ;
#7530 = CARTESIAN_POINT ( 'NONE',  ( -19.99999999999999645, -9.000000000000003553, 5.000000000000079936 ) ) ;
#7531 = CARTESIAN_POINT ( 'NONE',  ( 70.70000000109247651, 9.143825827087049163, 17.06698729999999742 ) ) ;
#7532 = ORIENTED_EDGE ( 'NONE', *, *, #21343, .T. ) ;
#7533 = CARTESIAN_POINT ( 'NONE',  ( -1.656854249492380138, -3.999999999999999112, 11.18750000000000888 ) ) ;
#7534 = CARTESIAN_POINT ( 'NONE',  ( 55.00000000000000711, 15.00000000000000000, 10.00000000000000000 ) ) ;
#7535 = CARTESIAN_POINT ( 'NONE',  ( 55.65393183416158251, 5.971812294485358663, 16.58880310854675599 ) ) ;
#7536 = DIRECTION ( 'NONE',  ( 1.000000000000000000, 7.703719777548943412E-32, 0.000000000000000000 ) ) ;
#7537 = CARTESIAN_POINT ( 'NONE',  ( -0.3649867057748841237, 3.983313282257322285, -19.99999999999999289 ) ) ;
#7538 = DIRECTION ( 'NONE',  ( 6.123233995736706871E-17, 0.8660254037844414832, 0.4999999999999951705 ) ) ;
#7539 = CARTESIAN_POINT ( 'NONE',  ( 4.000000000000000888, -0.8578082829538523635, -3.433262215449808696 ) ) ;
#7540 = ORIENTED_EDGE ( 'NONE', *, *, #18829, .T. ) ;
#7541 = CARTESIAN_POINT ( 'NONE',  ( 2.499999999999999556, -1.464956435139468161, -10.90201369670500497 ) ) ;
#7542 = CARTESIAN_POINT ( 'NONE',  ( -4.197312064133472020, -0.8182229787990021874, -3.502518405183886685 ) ) ;
#7543 = DIRECTION ( 'NONE',  ( 0.000000000000000000, 0.000000000000000000, 1.000000000000000000 ) ) ;
#7544 = ORIENTED_EDGE ( 'NONE', *, *, #19308, .F. ) ;
#7545 = LINE ( 'NONE', #23587, #20070 ) ;
#7546 = CARTESIAN_POINT ( 'NONE',  ( 47.23681404676619877, -9.000000000000001776, 10.00000000000008882 ) ) ;
#7547 = FACE_BOUND ( 'NONE', #731, .T. ) ;
#7548 = DIRECTION ( 'NONE',  ( 0.000000000000000000, 0.000000000000000000, 1.000000000000000000 ) ) ;
#7549 = ORIENTED_EDGE ( 'NONE', *, *, #6167, .F. ) ;
#7550 = CARTESIAN_POINT ( 'NONE',  ( 70.09999999999999432, 9.999999999999998224, 17.49999999999999645 ) ) ;
#7551 = ORIENTED_EDGE ( 'NONE', *, *, #17410, .T. ) ;
#7552 = FACE_OUTER_BOUND ( 'NONE', #3120, .T. ) ;
#7553 = VECTOR ( 'NONE', #7485, 1000.000000000000000 ) ;
#7554 = CARTESIAN_POINT ( 'NONE',  ( -3.999999999999999112, 1.656854249492380804, 14.93750000000000888 ) ) ;
#7555 = CARTESIAN_POINT ( 'NONE',  ( -4.350525068611870161, 4.993776679985856504, -3.644669744206380013 ) ) ;
#7556 = TOROIDAL_SURFACE ( 'NONE', #14073, 8.239200000000002078, 0.03079999999999868954 ) ;
#7557 = CARTESIAN_POINT ( 'NONE',  ( 65.85000000109246798, 9.999999999999998224, 17.06698730000000097 ) ) ;
#7558 =( BOUNDED_CURVE ( )  B_SPLINE_CURVE ( 2, ( #23085, #6696, #15922, #14133, #4657, #11991, #19259, #9223, #23332 ),
 .UNSPECIFIED., .F., .F. ) 
 B_SPLINE_CURVE_WITH_KNOTS ( ( 3, 2, 2, 2, 3 ),
 ( 0.3499999999999999778, 0.3624999999999999889, 0.3750000000000000000, 0.3875000000000000111, 0.4000000000000000222 ),
 .UNSPECIFIED. ) 
 CURVE ( )  GEOMETRIC_REPRESENTATION_ITEM ( )  RATIONAL_B_SPLINE_CURVE ( ( 1.000000000000000000, 0.9238795325112867385, 1.000000000000000000, 0.9238795325112867385, 1.000000000000000000, 0.9238795325112867385, 1.000000000000000000, 0.9238795325112867385, 1.000000000000000000 ) ) 
 REPRESENTATION_ITEM ( '' )  );
#7559 = CARTESIAN_POINT ( 'NONE',  ( -3.999999999999999112, 1.656854249492380582, 18.06250000273119483 ) ) ;
#7560 = CARTESIAN_POINT ( 'NONE',  ( 71.55000000109245661, 8.538419263543522320, 16.46158073645647235 ) ) ;
#7561 = EDGE_LOOP ( 'NONE', ( #21811, #7181 ) ) ;
#7562 = VECTOR ( 'NONE', #20416, 999.9999999999997726 ) ;
#7563 = VECTOR ( 'NONE', #168, 1000.000000000000114 ) ;
#7564 = CARTESIAN_POINT ( 'NONE',  ( 2.499999999999999556, 9.680994141368771011, 5.222868219166890036 ) ) ;
#7565 = CARTESIAN_POINT ( 'NONE',  ( 1.656854249492383024, -3.999999999999999112, -0.2624999972688121797 ) ) ;
#7566 = CARTESIAN_POINT ( 'NONE',  ( 72.10000000109246798, 12.06698730000000275, 15.85617417291294196 ) ) ;
#7567 = CARTESIAN_POINT ( 'NONE',  ( 1.872352939448454495E-15, -3.458734125000000326, 17.68750000136560274 ) ) ;
#7568 = DIRECTION ( 'NONE',  ( -0.000000000000000000, -0.000000000000000000, 1.000000000000000000 ) ) ;
#7569 = ADVANCED_FACE ( 'NONE', ( #10544 ), #21390, .F. ) ;
#7570 = CARTESIAN_POINT ( 'NONE',  ( -3.458734125000000326, -1.432654583217642497, -1.949999998634404319 ) ) ;
#7571 = CARTESIAN_POINT ( 'NONE',  ( 4.000000000000000000, 1.656854249492381248, 4.862500000000001599 ) ) ;
#7572 = CARTESIAN_POINT ( 'NONE',  ( -71.40000000218495302, 9.999999999999998224, 12.49999999999999289 ) ) ;
#7573 = CARTESIAN_POINT ( 'NONE',  ( 1.432654583217641164, 3.458734125000000326, 14.12500000136560452 ) ) ;
#7574 = FACE_OUTER_BOUND ( 'NONE', #1581, .T. ) ;
#7575 = VERTEX_POINT ( 'NONE', #19600 ) ;
#7576 = CIRCLE ( 'NONE', #23628, 4.000000000000000000 ) ;
#7577 = CARTESIAN_POINT ( 'NONE',  ( -70.25000000109247367, 12.06698730000000097, 14.99999999999999645 ) ) ;
#7578 = ORIENTED_EDGE ( 'NONE', *, *, #4930, .F. ) ;
#7579 = CARTESIAN_POINT ( 'NONE',  ( 57.28125000000000711, 8.343145750507600766, 11.00000000000000533 ) ) ;
#7580 = CARTESIAN_POINT ( 'NONE',  ( -69.55000000109247082, 11.46158073645647235, 13.53841926354352232 ) ) ;
#7581 = APPLICATION_PROTOCOL_DEFINITION ( 'draft international standard', 'automotive_design', 1998, #3943 ) ;
#7582 = CARTESIAN_POINT ( 'NONE',  ( 7.001720609283449193, -8.974600000000002353, 5.000000000000079936 ) ) ;
#7583 = EDGE_LOOP ( 'NONE', ( #7401, #6309, #23451, #19227 ) ) ;
#7584 = AXIS2_PLACEMENT_3D ( 'NONE', #3531, #5088, #3414 ) ;
#7585 = VECTOR ( 'NONE', #23495, 1000.000000000000114 ) ;
#7586 = EDGE_LOOP ( 'NONE', ( #4546, #4744, #19169, #17631 ) ) ;
#7587 = CARTESIAN_POINT ( 'NONE',  ( -2.445694354108818303, -2.445694354108820967, 15.81250000136560629 ) ) ;
#7588 = CARTESIAN_POINT ( 'NONE',  ( 54.37500000000000711, 7.878679656440349177, 12.87867965644035984 ) ) ;
#7589 = CARTESIAN_POINT ( 'NONE',  ( -69.90000000109247935, 7.933012699999995476, 14.14382582708705094 ) ) ;
#7590 = CARTESIAN_POINT ( 'NONE',  ( -69.70000000109246230, 12.06698730000000275, 15.85617417291294196 ) ) ;
#7591 = CARTESIAN_POINT ( 'NONE',  ( -3.458734124999998105, -1.432654583217642497, 11.75000000136560629 ) ) ;
#7592 = LINE ( 'NONE', #14914, #378 ) ;
#7593 = CARTESIAN_POINT ( 'NONE',  ( 59.87268183416157541, 7.926799079670491466, 12.83056023321021755 ) ) ;
#7594 = CARTESIAN_POINT ( 'NONE',  ( 72.09999999999999432, 9.999999999999998224, 12.49999999999999289 ) ) ;
#7595 = CIRCLE ( 'NONE', #21722, 4.000000000000000888 ) ;
#7596 = EDGE_CURVE ( 'NONE', #10540, #1478, #13233, .T. ) ;
#7597 = CONICAL_SURFACE ( 'NONE', #8356, 6.543750000000017053, 0.4459949661726622105 ) ;
#7598 =( GEOMETRIC_REPRESENTATION_CONTEXT ( 3 ) GLOBAL_UNCERTAINTY_ASSIGNED_CONTEXT ( ( #6197 ) ) GLOBAL_UNIT_ASSIGNED_CONTEXT ( ( #6630, #19544, #12278 ) ) REPRESENTATION_CONTEXT ( 'NONE', 'WORKASPACE' ) );
#7599 = CARTESIAN_POINT ( 'NONE',  ( -3.458734125000000770, 0.000000000000000000, 5.987500001365596347 ) ) ;
#7600 = ADVANCED_FACE ( 'NONE', ( #22816 ), #2458, .T. ) ;
#7601 = CARTESIAN_POINT ( 'NONE',  ( -3.458734124999998105, -1.432654583217642275, 11.50000000136560452 ) ) ;
#7602 = CARTESIAN_POINT ( 'NONE',  ( -3.999999999999998224, -1.656854249492383246, 16.18750000273119838 ) ) ;
#7603 = CARTESIAN_POINT ( 'NONE',  ( -69.30000000218494449, 11.76776695296636888, 16.76776695296636532 ) ) ;
#7604 = ORIENTED_EDGE ( 'NONE', *, *, #11605, .F. ) ;
#7605 = CARTESIAN_POINT ( 'NONE',  ( 0.000000000000000000, -9.314797388894900720, 1.239665997526853580 ) ) ;
#7606 = FACE_OUTER_BOUND ( 'NONE', #2102, .T. ) ;
#7607 = ORIENTED_EDGE ( 'NONE', *, *, #22460, .T. ) ;
#7608 = CARTESIAN_POINT ( 'NONE',  ( 55.59375000000000711, 11.24264068711927322, 11.99999999999998934 ) ) ;
#7609 = CARTESIAN_POINT ( 'NONE',  ( 2.445694354108820523, -2.445694354108820079, 4.112500001365594571 ) ) ;
#7610 = EDGE_CURVE ( 'NONE', #8473, #589, #2704, .T. ) ;
#7611 = DIRECTION ( 'NONE',  ( -0.000000000000000000, -0.000000000000000000, 1.000000000000000000 ) ) ;
#7612 = VERTEX_POINT ( 'NONE', #8236 ) ;
#7613 = CARTESIAN_POINT ( 'NONE',  ( -1.656854249492380138, -3.999999999999999112, 13.18750000000001243 ) ) ;
#7614 = AXIS2_PLACEMENT_3D ( 'NONE', #17363, #19257, #20919 ) ;
#7615 = CARTESIAN_POINT ( 'NONE',  ( -19.99999999999999645, -15.00000000000001954, 5.000000000000079936 ) ) ;
#7616 = CARTESIAN_POINT ( 'NONE',  ( 2.500000000000000000, 0.000000000000000000, 0.000000000000000000 ) ) ;
#7617 = VERTEX_POINT ( 'NONE', #15556 ) ;
#7618 = PRODUCT_DEFINITION_SHAPE ( 'NONE', 'NONE',  #2996 ) ;
#7619 = FACE_OUTER_BOUND ( 'NONE', #1340, .T. ) ;
#7620 = DIRECTION ( 'NONE',  ( 0.000000000000000000, 0.8090169943749444537, 0.5877852522924770229 ) ) ;
#7621 = CARTESIAN_POINT ( 'NONE',  ( 69.34999999999999432, 8.964466094067258695, 17.50000000000000355 ) ) ;
#7622 = EDGE_CURVE ( 'NONE', #21366, #6714, #20780, .T. ) ;
#7623 = VECTOR ( 'NONE', #1204, 999.9999999999998863 ) ;
#7624 = CARTESIAN_POINT ( 'NONE',  ( 118.3095189484530181, -10.00000000000001954, 15.00000000000002842 ) ) ;
#7625 = AXIS2_PLACEMENT_3D ( 'NONE', #13725, #19092, #11586 ) ;
#7626 = DIRECTION ( 'NONE',  ( 0.000000000000000000, 0.000000000000000000, 1.000000000000000000 ) ) ;
#7627 = CARTESIAN_POINT ( 'NONE',  ( 58.81481816583843170, 12.99999999999999822, 14.93194885905435676 ) ) ;
#7628 = EDGE_CURVE ( 'NONE', #22527, #6569, #6313, .T. ) ;
#7629 = CARTESIAN_POINT ( 'NONE',  ( -2.445694354108819635, -2.445694354108820523, 1.862500001365596347 ) ) ;
#7630 = CARTESIAN_POINT ( 'NONE',  ( 2.445694354108821411, 2.445694354108820523, 13.31250000136560452 ) ) ;
#7631 = DIRECTION ( 'NONE',  ( -1.000000000000000000, 0.000000000000000000, 0.000000000000000000 ) ) ;
#7632 = LINE ( 'NONE', #4136, #23140 ) ;
#7633 = AXIS2_PLACEMENT_3D ( 'NONE', #3607, #5297, #10481 ) ;
#7634 = FACE_OUTER_BOUND ( 'NONE', #3971, .T. ) ;
#7635 = ORIENTED_EDGE ( 'NONE', *, *, #6308, .F. ) ;
#7636 = DIRECTION ( 'NONE',  ( 0.9396926207859107594, -0.3420201433256623291, 3.697785493223492838E-32 ) ) ;
#7637 = AXIS2_PLACEMENT_3D ( 'NONE', #9202, #6919, #20167 ) ;
#7638 = DIRECTION ( 'NONE',  ( 0.000000000000000000, 0.000000000000000000, 1.000000000000000000 ) ) ;
#7639 = DIRECTION ( 'NONE',  ( 0.000000000000000000, 0.000000000000000000, 1.000000000000000000 ) ) ;
#7640 = ADVANCED_FACE ( 'NONE', ( #4501 ), #8125, .F. ) ;
#7641 = ORIENTED_EDGE ( 'NONE', *, *, #17516, .F. ) ;
#7642 = ADVANCED_FACE ( 'NONE', ( #548 ), #15435, .T. ) ;
#7643 =( REPRESENTATION_RELATIONSHIP ('NONE','NONE', #8403, #15757 ) REPRESENTATION_RELATIONSHIP_WITH_TRANSFORMATION ( #19392 )SHAPE_REPRESENTATION_RELATIONSHIP( ) );
#7644 = ORIENTED_EDGE ( 'NONE', *, *, #6969, .T. ) ;
#7645 = AXIS2_PLACEMENT_3D ( 'NONE', #2964, #13789, #8511 ) ;
#7646 = CARTESIAN_POINT ( 'NONE',  ( 53.62500000000000711, 12.82842712474620228, 17.82842712474617386 ) ) ;
#7647 = VERTEX_POINT ( 'NONE', #17090 ) ;
#7648 = CARTESIAN_POINT ( 'NONE',  ( 12.67929489676620314, -9.000000000000005329, 10.00000000000008882 ) ) ;
#7649 = ORIENTED_EDGE ( 'NONE', *, *, #12863, .F. ) ;
#7650 = AXIS2_PLACEMENT_3D ( 'NONE', #1284, #937, #6353 ) ;
#7651 = CARTESIAN_POINT ( 'NONE',  ( 54.12731816583844591, 12.87654654797634102, 17.78030770151602979 ) ) ;
#7652 = CARTESIAN_POINT ( 'NONE',  ( 70.20000000109246230, 12.06698730000000275, 14.14382582708705094 ) ) ;
#7653 = DIRECTION ( 'NONE',  ( -1.000000000000000000, 0.000000000000000000, 0.000000000000000000 ) ) ;
#7654 = ORIENTED_EDGE ( 'NONE', *, *, #20761, .F. ) ;
#7655 = CARTESIAN_POINT ( 'NONE',  ( 4.000000000000000888, 4.898587196589412829E-16, 16.62500000273119838 ) ) ;
#7656 = CARTESIAN_POINT ( 'NONE',  ( 1.600000000000004086, 1.012170579495290078E-15, 8.265000000000021885 ) ) ;
#7657 = CARTESIAN_POINT ( 'NONE',  ( 54.15393183416158251, 5.971812294485358663, 16.58880310854675599 ) ) ;
#7658 = CARTESIAN_POINT ( 'NONE',  ( 3.280735753986837366, -1.667205581200902120, 2.040000000000033786 ) ) ;
#7659 = CARTESIAN_POINT ( 'NONE',  ( 45.00000000000000000, -9.796556200126378400, 10.00000000000008882 ) ) ;
#7660 = CIRCLE ( 'NONE', #14179, 11.00000000000000000 ) ;
#7661 = DIRECTION ( 'NONE',  ( 0.000000000000000000, 0.000000000000000000, 1.000000000000000000 ) ) ;
#7662 = AXIS2_PLACEMENT_3D ( 'NONE', #7032, #14705, #21961 ) ;
#7663 = CARTESIAN_POINT ( 'NONE',  ( 8.718769219667262149, -11.25000000000000355, 5.000000000000079936 ) ) ;
#7664 = CARTESIAN_POINT ( 'NONE',  ( 4.350525068611871049, -4.993776679985862721, -3.644669744206375572 ) ) ;
#7665 = VERTEX_POINT ( 'NONE', #5949 ) ;
#7667 = EDGE_CURVE ( 'NONE', #16157, #10374, #11840, .T. ) ;
#7666 = CARTESIAN_POINT ( 'NONE',  ( 4.999999999999999112, -0.4999240074893842034, -8.734705317681632053 ) ) ;
#7668 = CARTESIAN_POINT ( 'NONE',  ( -4.000000000000000000, -2.472261339043343220, -3.687027428081192326 ) ) ;
#7669 = CYLINDRICAL_SURFACE ( 'NONE', #8959, 4.000000000000001776 ) ;
#7670 =( LENGTH_UNIT ( ) NAMED_UNIT ( * ) SI_UNIT ( .MILLI., .METRE. ) );
#7671 = EDGE_CURVE ( 'NONE', #22394, #14554, #4147, .T. ) ;
#7672 = TOROIDAL_SURFACE ( 'NONE', #18368, 6.200000000000021494, 0.1999999999999996503 ) ;
#7673 = EDGE_CURVE ( 'NONE', #12363, #7665, #23635, .T. ) ;
#7674 = ORIENTED_EDGE ( 'NONE', *, *, #15078, .T. ) ;
#7675 = LINE ( 'NONE', #21890, #5932 ) ;
#7676 = DIRECTION ( 'NONE',  ( 7.087422195345011518E-32, 1.000000000000000000, -0.000000000000000000 ) ) ;
#7677 = DIRECTION ( 'NONE',  ( 1.000000000000000000, 0.000000000000000000, 0.000000000000000000 ) ) ;
#7678 = VECTOR ( 'NONE', #20739, 1000.000000000000000 ) ;
#7679 = FACE_OUTER_BOUND ( 'NONE', #8704, .T. ) ;
#7680 = VERTEX_POINT ( 'NONE', #15320 ) ;
#7681 = CARTESIAN_POINT ( 'NONE',  ( 27.50000000000000000, 7.500000000000001776, -33.66025403784446723 ) ) ;
#7682 = ORIENTED_EDGE ( 'NONE', *, *, #17141, .T. ) ;
#7683 = CYLINDRICAL_SURFACE ( 'NONE', #1460, 4.000000000000000000 ) ;
#7684 = CARTESIAN_POINT ( 'NONE',  ( 1.656854249492381470, 4.000000000000000000, 14.68750000000000888 ) ) ;
#7685 = CARTESIAN_POINT ( 'NONE',  ( 4.999999999999997335, 0.000000000000000000, 0.000000000000000000 ) ) ;
#7686 = DIRECTION ( 'NONE',  ( 0.000000000000000000, 0.000000000000000000, 1.000000000000000000 ) ) ;
#7687 = CARTESIAN_POINT ( 'NONE',  ( 25.25491034071656316, -8.974600000000002353, 5.000000000000079936 ) ) ;
#7688 = CARTESIAN_POINT ( 'NONE',  ( 69.70000000109247651, 12.06698729999999919, 15.85617417291294196 ) ) ;
#7689 = VERTEX_POINT ( 'NONE', #22455 ) ;
#7690 = CIRCLE ( 'NONE', #7315, 4.250000000000000000 ) ;
#7691 = DIRECTION ( 'NONE',  ( 0.000000000000000000, 0.000000000000000000, -1.000000000000000000 ) ) ;
#7692 = AXIS2_PLACEMENT_3D ( 'NONE', #13679, #12008, #13806 ) ;
#7693 = CARTESIAN_POINT ( 'NONE',  ( 4.999999999999999112, 9.241976615262160522, -1.699438267350405818 ) ) ;
#7694 = CARTESIAN_POINT ( 'NONE',  ( 65.70000000109249072, 9.143825827087049163, 17.06698729999999742 ) ) ;
#7695 = CARTESIAN_POINT ( 'NONE',  ( -3.458734124999998993, -1.432654583217642497, 18.50000000136560629 ) ) ;
#7696 = FACE_OUTER_BOUND ( 'NONE', #18578, .T. ) ;
#7697 = CARTESIAN_POINT ( 'NONE',  ( 25.00005080000000035, 3.872983346207417021, -1.000000000000000000 ) ) ;
#7698 = CARTESIAN_POINT ( 'NONE',  ( -2.828427124746189403, -2.828427124746190735, 1.425000000000000933 ) ) ;
#7699 = CYLINDRICAL_SURFACE ( 'NONE', #11221, 4.000000000000001776 ) ;
#7700 = CARTESIAN_POINT ( 'NONE',  ( -2.445694354108819191, 2.445694354108820523, 12.31250000136560629 ) ) ;
#7701 = CARTESIAN_POINT ( 'NONE',  ( 4.999999999999999112, 0.000000000000000000, 0.000000000000000000 ) ) ;
#7702 = ORIENTED_EDGE ( 'NONE', *, *, #13918, .F. ) ;
#7703 = CARTESIAN_POINT ( 'NONE',  ( -67.75000000109247367, 11.46158073645647235, 13.53841926354352232 ) ) ;
#7704 = ORIENTED_EDGE ( 'NONE', *, *, #9384, .F. ) ;
#7705 = CARTESIAN_POINT ( 'NONE',  ( 58.03125000000000711, 11.65685424949239923, 18.99999999999998934 ) ) ;
#7706 = CARTESIAN_POINT ( 'NONE',  ( -71.85000000109246798, 9.999999999999998224, 12.93301269999999192 ) ) ;
#7707 = PRODUCT_CONTEXT ( 'NONE', #8871, 'mechanical' ) ;
#7708 = ORIENTED_EDGE ( 'NONE', *, *, #8808, .F. ) ;
#7709 = PLANE ( 'NONE',  #197 ) ;
#7710 = VERTEX_POINT ( 'NONE', #22590 ) ;
#7711 = AXIS2_PLACEMENT_3D ( 'NONE', #9337, #3570, #18417 ) ;
#7712 = VERTEX_POINT ( 'NONE', #6067 ) ;
#7713 = CARTESIAN_POINT ( 'NONE',  ( -2.445694354108818303, -2.445694354108820967, 18.81250000136560629 ) ) ;
#7714 = CARTESIAN_POINT ( 'NONE',  ( 53.06250000000000711, 6.999999999999997335, 15.00000000000000533 ) ) ;
#7715 = ADVANCED_FACE ( 'NONE', ( #21479 ), #15668, .F. ) ;
#7716 = CARTESIAN_POINT ( 'NONE',  ( -67.10000000109248219, 12.06698730000000275, 15.85617417291294196 ) ) ;
#7717 = CARTESIAN_POINT ( 'NONE',  ( 68.70000000109247651, 12.06698729999999919, 15.85617417291294196 ) ) ;
#7718 = B_SPLINE_CURVE_WITH_KNOTS ( 'NONE', 3,
 ( #12825, #16752, #9587, #7664, #9342, #16879 ),
 .UNSPECIFIED., .F., .F.,
 ( 4, 2, 4 ),
 ( 2.380733003149452133E-07, 0.001898835937927375499, 0.003797433802554436334 ),
 .UNSPECIFIED. ) ;
#7719 = CARTESIAN_POINT ( 'NONE',  ( -68.20000000109246230, 10.85617417291294551, 17.06698729999999742 ) ) ;
#7720 = CARTESIAN_POINT ( 'NONE',  ( 1.432654583217643163, -3.458734124999999882, 12.00000000136560807 ) ) ;
#7721 = DIRECTION ( 'NONE',  ( -1.000000000000000000, -0.000000000000000000, 0.000000000000000000 ) ) ;
#7722 = CARTESIAN_POINT ( 'NONE',  ( 57.99768183416157541, 12.16943976678977535, 12.92679907967048614 ) ) ;
#7723 = FACE_OUTER_BOUND ( 'NONE', #4309, .T. ) ;
#7724 = CARTESIAN_POINT ( 'NONE',  ( 52.40625000000000000, 12.99999999999999645, 13.75735931288070191 ) ) ;
#7725 = DIRECTION ( 'NONE',  ( 0.3420201433256622181, 0.9396926207859107594, -6.162975822039141593E-32 ) ) ;
#7726 = CARTESIAN_POINT ( 'NONE',  ( 4.000000000000000888, 1.656854249492381248, 14.68750000273119660 ) ) ;
#7727 = CARTESIAN_POINT ( 'NONE',  ( 33.85151041966726382, -11.25000000000000355, 10.00000000000008882 ) ) ;
#7728 = ORIENTED_EDGE ( 'NONE', *, *, #441, .T. ) ;
#7729 = CARTESIAN_POINT ( 'NONE',  ( 19.99999999999999645, 1.500000000000003109, -50.00000000000000000 ) ) ;
#7730 = CARTESIAN_POINT ( 'NONE',  ( -70.34999999999999432, 7.499999999999996447, 13.96446609406725514 ) ) ;
#7731 = ORIENTED_EDGE ( 'NONE', *, *, #1434, .T. ) ;
#7732 = CARTESIAN_POINT ( 'NONE',  ( 57.52893183416158962, 11.17458954617365663, 18.02818770551464311 ) ) ;
#7733 = CARTESIAN_POINT ( 'NONE',  ( 4.000000000000000888, -1.656854249492379694, -3.137499997268812901 ) ) ;
#7734 = CARTESIAN_POINT ( 'NONE',  ( 0.000000000000000000, 0.000000000000000000, -5.000000000000000000 ) ) ;
#7735 = ORIENTED_EDGE ( 'NONE', *, *, #20584, .T. ) ;
#7736 = CARTESIAN_POINT ( 'NONE',  ( 4.000000000000000888, 1.656854249492381248, 12.56250000000001243 ) ) ;
#7737 = DIRECTION ( 'NONE',  ( 0.000000000000000000, 0.000000000000000000, 1.000000000000000000 ) ) ;
#7738 = CARTESIAN_POINT ( 'NONE',  ( 4.999999999999999112, -1.699438267350438903, 9.241976615262153416 ) ) ;
#7739 = ORIENTED_EDGE ( 'NONE', *, *, #3220, .F. ) ;
#7740 = EDGE_CURVE ( 'NONE', #8014, #16322, #14877, .T. ) ;
#7741 = CARTESIAN_POINT ( 'NONE',  ( -70.95000000218495018, 11.03553390593273598, 17.50000000000000355 ) ) ;
#7742 = EDGE_CURVE ( 'NONE', #6426, #6127, #19690, .T. ) ;
#7743 = CARTESIAN_POINT ( 'NONE',  ( -3.458734125000000770, 1.432654583217640498, 0.9250000013655965692 ) ) ;
#7744 = CARTESIAN_POINT ( 'NONE',  ( 70.05000000000002558, 11.03553390593273598, 17.50000000000000355 ) ) ;
#7745 = EDGE_CURVE ( 'NONE', #22278, #20599, #10673, .T. ) ;
#7746 = LINE ( 'NONE', #22317, #21921 ) ;
#7747 = DIRECTION ( 'NONE',  ( 0.000000000000000000, 0.000000000000000000, -1.000000000000000000 ) ) ;
#7748 = CARTESIAN_POINT ( 'NONE',  ( 51.68981816583844591, 9.931948859054346102, 10.99999999999999467 ) ) ;
#7749 = CARTESIAN_POINT ( 'NONE',  ( -3.458734125000000770, 1.432654583217640498, 4.925000001365594571 ) ) ;
#7750 = CARTESIAN_POINT ( 'NONE',  ( -3.458734124999999437, 0.000000000000000000, 13.68750000136560629 ) ) ;
#7751 = CARTESIAN_POINT ( 'NONE',  ( 4.999999999999999112, 0.000000000000000000, 0.000000000000000000 ) ) ;
#7752 = DIRECTION ( 'NONE',  ( 0.000000000000000000, -1.000000000000000000, 0.000000000000000000 ) ) ;
#7753 = ORIENTED_EDGE ( 'NONE', *, *, #9366, .F. ) ;
#7754 = FACE_OUTER_BOUND ( 'NONE', #14602, .T. ) ;
#7755 = CARTESIAN_POINT ( 'NONE',  ( 2.000000000000005329, -3.464101615137751722, 0.000000000000000000 ) ) ;
#7756 = CARTESIAN_POINT ( 'NONE',  ( -70.80000000109248504, 9.143825827087050939, 12.93301269999999370 ) ) ;
#7757 = VERTEX_POINT ( 'NONE', #16129 ) ;
#7758 = EDGE_LOOP ( 'NONE', ( #11769, #5055, #3857, #11841 ) ) ;
#7759 = CYLINDRICAL_SURFACE ( 'NONE', #15987, 2.649999999999999467 ) ;
#7760 = CARTESIAN_POINT ( 'NONE',  ( 51.18750000000000711, 9.999999999999978684, 10.99999999999999645 ) ) ;
#7761 = VERTEX_POINT ( 'NONE', #19463 ) ;
#7762 = CARTESIAN_POINT ( 'NONE',  ( 2.712762565639649015, -3.052587955997662306, -3.430618716626630871 ) ) ;
#7763 = EDGE_LOOP ( 'NONE', ( #13689, #6480, #20356, #7285 ) ) ;
#7764 = CARTESIAN_POINT ( 'NONE',  ( 55.53356816583845301, 11.72490539043803004, 18.97181229448534268 ) ) ;
#7765 = EDGE_CURVE ( 'NONE', #5838, #6808, #3171, .T. ) ;
#7766 = EDGE_CURVE ( 'NONE', #3172, #13557, #7019, .T. ) ;
#7767 = CARTESIAN_POINT ( 'NONE',  ( 65.75000000218494733, 8.964466094067258695, 12.49999999999999289 ) ) ;
#7768 = DIRECTION ( 'NONE',  ( 1.000000000000000000, 0.000000000000000000, 0.000000000000000000 ) ) ;
#7769 = CARTESIAN_POINT ( 'NONE',  ( 70.10000000109245377, 7.933012699999995476, 14.14382582708705094 ) ) ;
#7770 = ADVANCED_FACE ( 'NONE', ( #3294 ), #14336, .T. ) ;
#7771 = ORIENTED_EDGE ( 'NONE', *, *, #18420, .T. ) ;
#7772 = CARTESIAN_POINT ( 'NONE',  ( -3.999999999999998224, -1.656854249492383246, 13.18750000273119660 ) ) ;
#7773 = EDGE_CURVE ( 'NONE', #2992, #14633, #6446, .T. ) ;
#7774 = CARTESIAN_POINT ( 'NONE',  ( -67.80000000218494449, 9.999999999999998224, 17.49999999999999645 ) ) ;
#7775 = CARTESIAN_POINT ( 'NONE',  ( 59.62500000000000711, 12.82842712474620228, 17.82842712474617386 ) ) ;
#7776 = CARTESIAN_POINT ( 'NONE',  ( 4.999999999999999112, -8.152713396088785203, 3.174628368996045946 ) ) ;
#7777 = DIRECTION ( 'NONE',  ( 0.000000000000000000, 0.000000000000000000, -1.000000000000000000 ) ) ;
#7778 = CARTESIAN_POINT ( 'NONE',  ( 25.00005080000000035, 5.400000000000000355, -1.000000000000000000 ) ) ;
#7779 = CARTESIAN_POINT ( 'NONE',  ( -67.25000000109245946, 12.06698730000000097, 14.99999999999999645 ) ) ;
#7780 = CARTESIAN_POINT ( 'NONE',  ( -1.876855952934450622, 6.421950209808279908, -0.1061556211655337173 ) ) ;
#7781 = ORIENTED_EDGE ( 'NONE', *, *, #906, .F. ) ;
#7782 = CARTESIAN_POINT ( 'NONE',  ( 54.09375000000000711, 11.24264068711927322, 11.99999999999998934 ) ) ;
#7783 = DIRECTION ( 'NONE',  ( -1.000000000000000000, -7.703719777548943412E-32, 0.000000000000000000 ) ) ;
#7784 = ORIENTED_EDGE ( 'NONE', *, *, #23464, .F. ) ;
#7785 = CONICAL_SURFACE ( 'NONE', #21527, 6.500000000000000888, 1.047197551196596521 ) ;
#7786 = CARTESIAN_POINT ( 'NONE',  ( 69.10000000218495586, 11.76776695296636888, 13.23223304703362579 ) ) ;
#7787 = DIRECTION ( 'NONE',  ( 0.000000000000000000, 0.000000000000000000, 1.000000000000000000 ) ) ;
#7788 = CARTESIAN_POINT ( 'NONE',  ( 0.000000000000000000, 7.593217523260583413, 7.958834565716794707 ) ) ;
#7789 = AXIS2_PLACEMENT_3D ( 'NONE', #970, #4227, #9871 ) ;
#7790 = DIRECTION ( 'NONE',  ( -1.000000000000000000, 0.000000000000000000, 0.000000000000000000 ) ) ;
#7791 = VERTEX_POINT ( 'NONE', #17796 ) ;
#7792 = DIRECTION ( 'NONE',  ( 0.000000000000000000, 0.000000000000000000, -1.000000000000000000 ) ) ;
#7793 = ORIENTED_EDGE ( 'NONE', *, *, #3510, .T. ) ;
#7794 = CARTESIAN_POINT ( 'NONE',  ( -12.44420145928343935, -8.974600000000002353, 10.00000000000008882 ) ) ;
#7795 = EDGE_CURVE ( 'NONE', #3403, #22760, #22880, .T. ) ;
#7796 = CARTESIAN_POINT ( 'NONE',  ( 4.000000000000001776, -1.656854249492379694, 15.43750000000001066 ) ) ;
#7797 = DIRECTION ( 'NONE',  ( 1.000000000000000000, 0.000000000000000000, 0.000000000000000000 ) ) ;
#7798 = CARTESIAN_POINT ( 'NONE',  ( 6.500000000000000000, 0.6345343291280540754, -3.700000000000000178 ) ) ;
#7799 = CARTESIAN_POINT ( 'NONE',  ( 71.65000000109246514, 7.933012699999995476, 14.99999999999999645 ) ) ;
#7800 = ORIENTED_EDGE ( 'NONE', *, *, #5730, .T. ) ;
#7801 = EDGE_CURVE ( 'NONE', #7712, #1981, #5210, .T. ) ;
#7802 = VECTOR ( 'NONE', #2080, 1000.000000000000000 ) ;
#7803 = CARTESIAN_POINT ( 'NONE',  ( 3.250000000000001776, -5.629165124598848990, 1.734723475976807094E-15 ) ) ;
#7804 = DIRECTION ( 'NONE',  ( 0.000000000000000000, 0.3090169943749481174, -0.9510565162951533091 ) ) ;
#7805 = CARTESIAN_POINT ( 'NONE',  ( 66.35000000109248219, 11.46158073645647235, 16.46158073645647235 ) ) ;
#7806 = CARTESIAN_POINT ( 'NONE',  ( -3.458734124999998993, 0.000000000000000000, 15.43750000136560452 ) ) ;
#7807 = CYLINDRICAL_SURFACE ( 'NONE', #19290, 11.00000000000000000 ) ;
#7808 = CARTESIAN_POINT ( 'NONE',  ( -3.458734125000000770, 0.000000000000000000, -1.012499998634402543 ) ) ;
#7809 = CARTESIAN_POINT ( 'NONE',  ( 1.656854249492383024, -3.999999999999999112, 0.6125000000000022649 ) ) ;
#7810 = CARTESIAN_POINT ( 'NONE',  ( -19.99999999999999645, -9.000000000000003553, 10.00000000000008882 ) ) ;
#7811 = CARTESIAN_POINT ( 'NONE',  ( 1.432654583217643163, -3.458734124999999437, 13.75000000136560452 ) ) ;
#7812 = CARTESIAN_POINT ( 'NONE',  ( 72.50000000000000000, 9.999999999999998224, 14.99999999999999645 ) ) ;
#7813 = EDGE_LOOP ( 'NONE', ( #21292, #4207, #9055, #8498 ) ) ;
#7814 = CARTESIAN_POINT ( 'NONE',  ( -1.656854249492379472, 4.000000000000000000, 15.93750000273119838 ) ) ;
#7815 = VERTEX_POINT ( 'NONE', #21359 ) ;
#7816 = CARTESIAN_POINT ( 'NONE',  ( 56.25000000000000711, 7.171572875253819923, 17.82842712474619873 ) ) ;
#7817 = CARTESIAN_POINT ( 'NONE',  ( -72.10000000109246798, 12.06698730000000275, 15.85617417291294196 ) ) ;
#7818 = APPLICATION_PROTOCOL_DEFINITION ( 'draft international standard', 'automotive_design', 1998, #14678 ) ;
#7819 = ORIENTED_EDGE ( 'NONE', *, *, #7209, .T. ) ;
#7820 = FACE_OUTER_BOUND ( 'NONE', #7295, .T. ) ;
#7821 = ORIENTED_EDGE ( 'NONE', *, *, #9071, .T. ) ;
#7822 = ORIENTED_EDGE ( 'NONE', *, *, #6263, .F. ) ;
#7823 = CARTESIAN_POINT ( 'NONE',  ( 1.025207404391860050E-15, 3.458734125000000770, 16.43750000136560629 ) ) ;
#7824 = CARTESIAN_POINT ( 'NONE',  ( 57.75000000000000000, 7.878679656440361612, 17.12132034355964549 ) ) ;
#7825 = CARTESIAN_POINT ( 'NONE',  ( -66.55000000109247082, 8.538419263543522320, 16.46158073645647235 ) ) ;
#7826 = CARTESIAN_POINT ( 'NONE',  ( 70.00000000109247367, 9.143825827087052716, 12.93301269999999192 ) ) ;
#7827 = ADVANCED_FACE ( 'NONE', ( #6778 ), #9515, .T. ) ;
#7828 = CARTESIAN_POINT ( 'NONE',  ( -66.95000000109246230, 8.538419263543524096, 13.53841926354352054 ) ) ;
#7829 = DIRECTION ( 'NONE',  ( 0.000000000000000000, 0.000000000000000000, -1.000000000000000000 ) ) ;
#7830 = CARTESIAN_POINT ( 'NONE',  ( 55.84143183416158251, 8.689308171935088865, 17.97181229448535689 ) ) ;
#7831 = CARTESIAN_POINT ( 'NONE',  ( 4.000000000000000000, 0.000000000000000000, 19.04999999999996874 ) ) ;
#7832 = CARTESIAN_POINT ( 'NONE',  ( -2.117863837641485618E-16, 3.458734125000000770, 2.737500001365597235 ) ) ;
#7833 = CARTESIAN_POINT ( 'NONE',  ( 2.445694354108821855, -2.445694354108820079, 12.81250000136560629 ) ) ;
#7834 = CARTESIAN_POINT ( 'NONE',  ( -1.656854249492380138, -3.999999999999999112, 14.31250000273119660 ) ) ;
#7835 = CARTESIAN_POINT ( 'NONE',  ( -69.10000000218495586, 11.76776695296636888, 13.23223304703362579 ) ) ;
#7836 = ORIENTED_EDGE ( 'NONE', *, *, #9794, .F. ) ;
#7837 = DIRECTION ( 'NONE',  ( -7.087422195345011518E-32, -1.000000000000000000, 0.000000000000000000 ) ) ;
#7838 = ORIENTED_EDGE ( 'NONE', *, *, #17416, .F. ) ;
#7839 = CARTESIAN_POINT ( 'NONE',  ( 55.56018183416157541, 7.000000000000000000, 14.93194885905437097 ) ) ;
#7840 = CARTESIAN_POINT ( 'NONE',  ( 1.432654583217639832, 3.458734125000000326, 3.425000001365596791 ) ) ;
#7841 = CARTESIAN_POINT ( 'NONE',  ( 65.00000000000000000, 9.999999999999998224, 19.99999999999999645 ) ) ;
#7842 = ORIENTED_EDGE ( 'NONE', *, *, #7745, .F. ) ;
#7843 = CARTESIAN_POINT ( 'NONE',  ( 4.000000000000000888, 1.656854249492381248, 11.56250000000001066 ) ) ;
#7844 = DIRECTION ( 'NONE',  ( -5.546678239835226120E-32, -0.3420201433256691015, -0.9396926207859083169 ) ) ;
#7845 = VECTOR ( 'NONE', #7837, 1000.000000000000000 ) ;
#7846 = VECTOR ( 'NONE', #2974, 1000.000000000000000 ) ;
#7847 = DIRECTION ( 'NONE',  ( 0.9396926207859107594, -0.3420201433256623291, 3.697785493223492838E-32 ) ) ;
#7848 = VERTEX_POINT ( 'NONE', #6554 ) ;
#7849 = CARTESIAN_POINT ( 'NONE',  ( -69.15000000218495302, 12.50000000000000000, 13.96446609406725869 ) ) ;
#7850 = CARTESIAN_POINT ( 'NONE',  ( 3.458734125000000770, 1.432654583217640498, -1.449999998634403875 ) ) ;
#7851 = CARTESIAN_POINT ( 'NONE',  ( 1.236993788156008760E-15, 0.000000000000000000, 21.31370849898476649 ) ) ;
#7852 = CARTESIAN_POINT ( 'NONE',  ( 69.54999999999999716, 7.499999999999995559, 13.96446609406725692 ) ) ;
#7853 = CARTESIAN_POINT ( 'NONE',  ( 50.00000000000000000, -10.00000000000001954, 17.50000000000002842 ) ) ;
#7855 = DIRECTION ( 'NONE',  ( 1.000000000000000000, -0.000000000000000000, -0.000000000000000000 ) ) ;
#7854 = VECTOR ( 'NONE', #16526, 1000.000000000000000 ) ;
#7856 = CARTESIAN_POINT ( 'NONE',  ( 55.81481816583843170, 12.99999999999999822, 14.93194885905435676 ) ) ;
#7857 = AXIS2_PLACEMENT_3D ( 'NONE', #9584, #4164, #11511 ) ;
#7858 = CARTESIAN_POINT ( 'NONE',  ( -2.445694354108820523, 2.445694354108820523, 3.862500001365594571 ) ) ;
#7859 = CARTESIAN_POINT ( 'NONE',  ( 1.432654583217643163, -3.458734124999999882, 15.00000000136560629 ) ) ;
#7860 = DIRECTION ( 'NONE',  ( 0.3420201433256622736, -0.9396926207859106484, -1.232595164407828100E-31 ) ) ;
#7861 = CARTESIAN_POINT ( 'NONE',  ( -71.80000000109245661, 9.143825827087052716, 12.93301269999999192 ) ) ;
#7862 = EDGE_CURVE ( 'NONE', #3012, #6076, #21446, .T. ) ;
#7863 = PLANE ( 'NONE',  #21227 ) ;
#7864 = ORIENTED_EDGE ( 'NONE', *, *, #3766, .F. ) ;
#7865 = CARTESIAN_POINT ( 'NONE',  ( 0.1750025118121568690, 4.719839900820621104, -3.469254087858248070 ) ) ;
#7866 = CARTESIAN_POINT ( 'NONE',  ( -4.000000000000000000, 0.000000000000000000, 4.425000002731186655 ) ) ;
#7867 = CARTESIAN_POINT ( 'NONE',  ( -70.65000000109247935, 7.933012699999995476, 14.99999999999999645 ) ) ;
#7868 = ORIENTED_EDGE ( 'NONE', *, *, #8593, .T. ) ;
#7869 = ORIENTED_EDGE ( 'NONE', *, *, #15276, .F. ) ;
#7870 =( NAMED_UNIT ( * ) SI_UNIT ( $, .STERADIAN. ) SOLID_ANGLE_UNIT ( ) );
#7871 = EDGE_CURVE ( 'NONE', #14298, #2537, #9897, .T. ) ;
#7872 = DIRECTION ( 'NONE',  ( 1.000000000000000000, -0.000000000000000000, -0.000000000000000000 ) ) ;
#7873 = ORIENTED_EDGE ( 'NONE', *, *, #119, .T. ) ;
#7874 = CARTESIAN_POINT ( 'NONE',  ( 4.999999999999999112, -5.222868219166784343, -9.680994141368826078 ) ) ;
#7875 = PRODUCT_DEFINITION_CONTEXT ( 'detailed design', #2718, 'design' ) ;
#7876 = AXIS2_PLACEMENT_3D ( 'NONE', #22878, #11667, #17153 ) ;
#7877 = AXIS2_PLACEMENT_3D ( 'NONE', #1152, #15798, #11856 ) ;
#7878 = CARTESIAN_POINT ( 'NONE',  ( 69.95000000109247651, 8.538419263543524096, 13.53841926354352054 ) ) ;
#7879 = CARTESIAN_POINT ( 'NONE',  ( 66.34999999999999432, 7.499999999999996447, 13.96446609406725514 ) ) ;
#7880 = CARTESIAN_POINT ( 'NONE',  ( 69.95000000109247651, 8.538419263543522320, 16.46158073645647235 ) ) ;
#7881 = ORIENTED_EDGE ( 'NONE', *, *, #10537, .T. ) ;
#7882 = CARTESIAN_POINT ( 'NONE',  ( -3.999999999999998224, -1.656854249492383246, 12.18750000273119838 ) ) ;
#7883 = AXIS2_PLACEMENT_3D ( 'NONE', #6798, #21382, #5003 ) ;
#7884 = DIRECTION ( 'NONE',  ( -0.7071067811865364705, 0.000000000000000000, 0.7071067811865584529 ) ) ;
#7885 = CARTESIAN_POINT ( 'NONE',  ( 55.84143183416158251, 8.275094609562001935, 18.97181229448536044 ) ) ;
#7886 = LINE ( 'NONE', #6080, #1175 ) ;
#7887 = CARTESIAN_POINT ( 'NONE',  ( -3.458734124999998993, 0.000000000000000000, 17.43750000136560274 ) ) ;
#7888 = LINE ( 'NONE', #11620, #21211 ) ;
#7889 = EDGE_CURVE ( 'NONE', #15752, #2469, #678, .T. ) ;
#7890 = CARTESIAN_POINT ( 'NONE',  ( -66.45000000109246230, 12.06698730000000097, 14.99999999999999645 ) ) ;
#7891 = ORIENTED_EDGE ( 'NONE', *, *, #1001, .F. ) ;
#7892 = CARTESIAN_POINT ( 'NONE',  ( 72.50000000000000000, 9.999999999999998224, 14.99999999999999645 ) ) ;
#7893 = ORIENTED_EDGE ( 'NONE', *, *, #13145, .F. ) ;
#7894 = EDGE_CURVE ( 'NONE', #1978, #5354, #6668, .T. ) ;
#7895 = CARTESIAN_POINT ( 'NONE',  ( 53.06250000000000711, 6.999999999999997335, 15.00000000000000533 ) ) ;
#7896 = DIRECTION ( 'NONE',  ( -0.000000000000000000, 1.000000000000000000, 1.224646799147353207E-16 ) ) ;
#7897 = ORIENTED_EDGE ( 'NONE', *, *, #10137, .F. ) ;
#7898 = CARTESIAN_POINT ( 'NONE',  ( 3.999999999999999112, 2.309401076758497595, -3.504271511726784194 ) ) ;
#7899 = DIRECTION ( 'NONE',  ( -1.000000000000000000, -0.000000000000000000, -0.000000000000000000 ) ) ;
#7900 = DIRECTION ( 'NONE',  ( 0.000000000000000000, 0.000000000000000000, 1.000000000000000000 ) ) ;
#7901 = ADVANCED_FACE ( 'NONE', ( #8585 ), #14223, .T. ) ;
#7902 = DIRECTION ( 'NONE',  ( 1.000000000000000000, 4.625929269271485914E-16, -1.224646799147353454E-16 ) ) ;
#7903 = ORIENTED_EDGE ( 'NONE', *, *, #22798, .T. ) ;
#7904 = CARTESIAN_POINT ( 'NONE',  ( 50.00000000000000000, -2.399706452296379577, 55.00000000000021316 ) ) ;
#7905 = ORIENTED_EDGE ( 'NONE', *, *, #20638, .T. ) ;
#7906 = CARTESIAN_POINT ( 'NONE',  ( 1.656854249492383024, -3.999999999999999112, 1.612500000000001377 ) ) ;
#7907 =( BOUNDED_CURVE ( )  B_SPLINE_CURVE ( 2, ( #9002, #14511, #21775, #16296, #3468, #5385, #12724, #1188, #15829 ),
 .UNSPECIFIED., .F., .F. ) 
 B_SPLINE_CURVE_WITH_KNOTS ( ( 3, 2, 2, 2, 3 ),
 ( 0.000000000000000000, 0.01562499999999990459, 0.03124999999999980918, 0.04687499999999971551, 0.06249999999999961836 ),
 .UNSPECIFIED. ) 
 CURVE ( )  GEOMETRIC_REPRESENTATION_ITEM ( )  RATIONAL_B_SPLINE_CURVE ( ( 1.000000000000000000, 0.9238795325112867385, 1.000000000000000000, 0.9238795325112867385, 1.000000000000000000, 0.9238795325112867385, 1.000000000000000000, 0.9238795325112886259, 0.9999999999999981126 ) ) 
 REPRESENTATION_ITEM ( '' )  );
#7908 = CARTESIAN_POINT ( 'NONE',  ( 9.920644283265380691E-16, 4.000000000000000000, 12.75000000000001066 ) ) ;
#7909 = FACE_OUTER_BOUND ( 'NONE', #18640, .T. ) ;
#7910 = ORIENTED_EDGE ( 'NONE', *, *, #8797, .F. ) ;
#7911 = CARTESIAN_POINT ( 'NONE',  ( 118.3095189484530181, -2.399706452296352932, 60.00000000000021316 ) ) ;
#7912 = FILL_AREA_STYLE_COLOUR ( '', #9473 ) ;
#7913 = CARTESIAN_POINT ( 'NONE',  ( 70.90000000109246514, 7.933012699999995476, 14.14382582708705094 ) ) ;
#7914 = ORIENTED_EDGE ( 'NONE', *, *, #20670, .T. ) ;
#7915 = CARTESIAN_POINT ( 'NONE',  ( -0.6666666666666651864, 4.233901974057260098, -3.300726591567081147 ) ) ;
#7916 = ADVANCED_FACE ( 'NONE', ( #12551 ), #23530, .F. ) ;
#7917 = FACE_OUTER_BOUND ( 'NONE', #17457, .T. ) ;
#7918 = CARTESIAN_POINT ( 'NONE',  ( 69.40000000109246514, 9.143825827087050939, 12.93301269999999370 ) ) ;
#7919 = CARTESIAN_POINT ( 'NONE',  ( -2.445694354108819191, 2.445694354108820523, 12.31250000136560629 ) ) ;
#7920 = CARTESIAN_POINT ( 'NONE',  ( 4.211140560182196957, -2.431303136016555122, -3.745885042887436622 ) ) ;
#7921 = DIRECTION ( 'NONE',  ( -1.000000000000000000, 0.000000000000000000, 1.224646799147353207E-16 ) ) ;
#7922 = CARTESIAN_POINT ( 'NONE',  ( -2.828427124746190291, 2.828427124746190291, 3.175000000000002487 ) ) ;
#7923 = ADVANCED_FACE ( 'NONE', ( #19813 ), #16241, .F. ) ;
#7924 = CARTESIAN_POINT ( 'NONE',  ( -2.828427124746189403, 2.828427124746190291, 12.87500000000001066 ) ) ;
#7925 = DIRECTION ( 'NONE',  ( 0.000000000000000000, 0.000000000000000000, -1.000000000000000000 ) ) ;
#7926 = DIRECTION ( 'NONE',  ( 0.000000000000000000, -0.000000000000000000, 1.000000000000000000 ) ) ;
#7927 = ORIENTED_EDGE ( 'NONE', *, *, #8075, .T. ) ;
#7928 = LINE ( 'NONE', #19168, #2844 ) ;
#7929 = VERTEX_POINT ( 'NONE', #9064 ) ;
#7930 = TOROIDAL_SURFACE ( 'NONE', #23594, 2.700000000000000622, 0.2000000000000000111 ) ;
#7931 = CARTESIAN_POINT ( 'NONE',  ( 56.71875000000000711, 14.00000000000000888, 16.65685424949235482 ) ) ;
#7932 = CARTESIAN_POINT ( 'NONE',  ( -67.55000000109247082, 8.538419263543522320, 16.46158073645647235 ) ) ;
#7933 = SHAPE_DEFINITION_REPRESENTATION ( #22708, #9307 ) ;
#7934 = ADVANCED_FACE ( 'NONE', ( #22062 ), #12784, .T. ) ;
#7935 = VERTEX_POINT ( 'NONE', #14454 ) ;
#7936 = DIRECTION ( 'NONE',  ( 0.3420201433256622181, 0.9396926207859107594, -6.162975822039141593E-32 ) ) ;
#7937 = VERTEX_POINT ( 'NONE', #7386 ) ;
#7938 = EDGE_CURVE ( 'NONE', #13486, #22180, #2220, .T. ) ;
#7939 = ORIENTED_EDGE ( 'NONE', *, *, #6324, .F. ) ;
#7940 = CARTESIAN_POINT ( 'NONE',  ( -3.458734124999999437, 1.432654583217640498, 17.62500000136560274 ) ) ;
#7941 = CARTESIAN_POINT ( 'NONE',  ( 58.59375000000000711, 11.24264068711927322, 11.99999999999998934 ) ) ;
#7942 = AXIS2_PLACEMENT_3D ( 'NONE', #10042, #4265, #22693 ) ;
#7943 = VECTOR ( 'NONE', #4418, 1000.000000000000000 ) ;
#7944 = CARTESIAN_POINT ( 'NONE',  ( -66.50000000109247367, 9.143825827087049163, 17.06698729999999742 ) ) ;
#7945 = CARTESIAN_POINT ( 'NONE',  ( 69.25000000109247367, 9.999999999999998224, 12.93301269999999192 ) ) ;
#7946 =( BOUNDED_CURVE ( )  B_SPLINE_CURVE ( 2, ( #12033, #4698, #22896, #2774, #19070, #13940, #2660, #13702, #17293 ),
 .UNSPECIFIED., .F., .F. ) 
 B_SPLINE_CURVE_WITH_KNOTS ( ( 3, 2, 2, 2, 3 ),
 ( 0.1249999999999992367, 0.1406249999999996947, 0.1562500000000001388, 0.1718750000000005829, 0.1875000000000010270 ),
 .UNSPECIFIED. ) 
 CURVE ( )  GEOMETRIC_REPRESENTATION_ITEM ( )  RATIONAL_B_SPLINE_CURVE ( ( 1.000000000000003775, 0.9238795325112830747, 1.000000000000000000, 0.9238795325112867385, 1.000000000000000000, 0.9238795325112867385, 1.000000000000000000, 0.9238795325112817425, 1.000000000000005107 ) ) 
 REPRESENTATION_ITEM ( '' )  );
#7947 = CARTESIAN_POINT ( 'NONE',  ( -72.00000000000000000, 8.232233047033629347, 13.23223304703362402 ) ) ;
#7948 = CARTESIAN_POINT ( 'NONE',  ( -2.423057340716551433, -8.974600000000002353, 5.000000000000079936 ) ) ;
#7949 = CARTESIAN_POINT ( 'NONE',  ( 54.06018183416157541, 7.000000000000000000, 14.93194885905437097 ) ) ;
#7950 = CARTESIAN_POINT ( 'NONE',  ( 60.00000000000000711, 12.12132034355963484, 12.87867965644034740 ) ) ;
#7951 =( REPRESENTATION_RELATIONSHIP ('NONE','NONE', #8403, #15757 ) REPRESENTATION_RELATIONSHIP_WITH_TRANSFORMATION ( #729 )SHAPE_REPRESENTATION_RELATIONSHIP( ) );
#7952 = CARTESIAN_POINT ( 'NONE',  ( 6.353591512924457348E-16, -3.458734125000000770, 5.237500001365596347 ) ) ;
#7953 = CARTESIAN_POINT ( 'NONE',  ( 3.458734125000002102, -1.432654583217639610, 10.87500000136560452 ) ) ;
#7954 = CARTESIAN_POINT ( 'NONE',  ( 4.000000000000000888, 1.656854249492381248, 11.68750000273119660 ) ) ;
#7955 = CARTESIAN_POINT ( 'NONE',  ( 3.333333333333332593, 2.694301256218250007, -3.300726591567078483 ) ) ;
#7956 = VECTOR ( 'NONE', #5008, 1000.000000000000000 ) ;
#7957 = ORIENTED_EDGE ( 'NONE', *, *, #11701, .F. ) ;
#7958 = DIRECTION ( 'NONE',  ( 0.000000000000000000, 0.000000000000000000, 1.000000000000000000 ) ) ;
#7959 = ORIENTED_EDGE ( 'NONE', *, *, #23411, .T. ) ;
#7960 = CARTESIAN_POINT ( 'NONE',  ( 57.24768183416158962, 7.830560233210222876, 17.07320092032950498 ) ) ;
#7961 = PRESENTATION_STYLE_ASSIGNMENT (( #4350 ) ) ;
#7962 = CARTESIAN_POINT ( 'NONE',  ( -2.117863837641485618E-16, 3.458734125000000326, 2.487500001365596791 ) ) ;
#7963 = EDGE_CURVE ( 'NONE', #5505, #11622, #4042, .T. ) ;
#7964 = CARTESIAN_POINT ( 'NONE',  ( -2.445694354108819635, -2.445694354108820523, -0.1374999986344035974 ) ) ;
#7965 = ORIENTED_EDGE ( 'NONE', *, *, #8208, .T. ) ;
#7966 = CARTESIAN_POINT ( 'NONE',  ( 1.656854249492384135, -3.999999999999999112, 11.31250000000001066 ) ) ;
#7967 = EDGE_CURVE ( 'NONE', #20452, #19427, #1727, .T. ) ;
#7968 = CYLINDRICAL_SURFACE ( 'NONE', #4898, 2.500000000000002220 ) ;
#7969 = CIRCLE ( 'NONE', #19424, 4.000000000000001776 ) ;
#7970 = LINE ( 'NONE', #15170, #2591 ) ;
#7971 = ORIENTED_EDGE ( 'NONE', *, *, #18837, .T. ) ;
#7972 = CIRCLE ( 'NONE', #17146, 6.000000000000000888 ) ;
#7973 = CARTESIAN_POINT ( 'NONE',  ( -70.85000000218494165, 12.50000000000000000, 16.03553390593273420 ) ) ;
#7974 = LINE ( 'NONE', #19207, #3328 ) ;
#7975 = VECTOR ( 'NONE', #18736, 1000.000000000000000 ) ;
#7976 = CARTESIAN_POINT ( 'NONE',  ( 60.00000000000000711, 15.00000000000000000, 10.00000000000007105 ) ) ;
#7977 = COLOUR_RGB ( '', 0.09019608, 0.27058824, 0.51372549) ;
#7978 = CARTESIAN_POINT ( 'NONE',  ( 66.84999999999999432, 11.03553390593273598, 17.50000000000000355 ) ) ;
#7979 = DIRECTION ( 'NONE',  ( 1.224646799147353207E-16, -0.000000000000000000, 1.000000000000000000 ) ) ;
#7980 = CARTESIAN_POINT ( 'NONE',  ( 70.20000000109246230, 12.06698730000000275, 14.14382582708705094 ) ) ;
#7981 = DIRECTION ( 'NONE',  ( 0.000000000000000000, 0.000000000000000000, -1.000000000000000000 ) ) ;
#7982 = CARTESIAN_POINT ( 'NONE',  ( 55.62731816583843170, 12.16943976678978601, 17.07320092032949432 ) ) ;
#7983 = CARTESIAN_POINT ( 'NONE',  ( 2.445694354108820079, 2.445694354108820523, 5.612500001365596347 ) ) ;
#7984 = CARTESIAN_POINT ( 'NONE',  ( 3.458734125000001658, 4.235727675282972223E-16, 16.18750000136560629 ) ) ;
#7985 = DIRECTION ( 'NONE',  ( 0.06805114094563521898, -0.7054675904022857935, -0.7054675904022735811 ) ) ;
#7986 = CARTESIAN_POINT ( 'NONE',  ( -71.55000000109245661, 8.538419263543522320, 16.46158073645647235 ) ) ;
#7987 = AXIS2_PLACEMENT_3D ( 'NONE', #1557, #14405, #3360 ) ;
#7988 = FACE_OUTER_BOUND ( 'NONE', #13994, .T. ) ;
#7989 = VERTEX_POINT ( 'NONE', #1723 ) ;
#7990 = CARTESIAN_POINT ( 'NONE',  ( -4.236525694536558362, 2.416953475386465211, -3.751298745799836354 ) ) ;
#7991 = CARTESIAN_POINT ( 'NONE',  ( 1.656854249492383024, -3.999999999999999112, 3.737500002731185766 ) ) ;
#7992 = CARTESIAN_POINT ( 'NONE',  ( -71.00000000109247367, 12.06698730000000275, 14.14382582708705094 ) ) ;
#7993 = VERTEX_POINT ( 'NONE', #16705 ) ;
#7994 = ORIENTED_EDGE ( 'NONE', *, *, #2231, .T. ) ;
#7995 = AXIS2_PLACEMENT_3D ( 'NONE', #9705, #4174, #572 ) ;
#7996 = DIRECTION ( 'NONE',  ( 0.000000000000000000, 0.000000000000000000, -1.000000000000000000 ) ) ;
#7997 = CARTESIAN_POINT ( 'NONE',  ( 1.077186599943259049, -1.328531455546325901, 10.00000000000008882 ) ) ;
#7998 = ORIENTED_EDGE ( 'NONE', *, *, #9997, .T. ) ;
#7999 = CARTESIAN_POINT ( 'NONE',  ( 4.141042297810615835, -2.227970268150433863, -3.687027686973623819 ) ) ;
#8000 = TOROIDAL_SURFACE ( 'NONE', #8770, 8.800000000000023803, 0.2000000000000000944 ) ;
#8001 = CARTESIAN_POINT ( 'NONE',  ( 68.55000000109247082, 11.46158073645647235, 13.53841926354352232 ) ) ;
#8002 = AXIS2_PLACEMENT_3D ( 'NONE', #22434, #17193, #771 ) ;
#8003 = ADVANCED_FACE ( 'NONE', ( #12893 ), #20150, .T. ) ;
#8004 = CARTESIAN_POINT ( 'NONE',  ( 69.25000000109245946, 7.933012699999995476, 14.99999999999999645 ) ) ;
#8005 = PRODUCT_DEFINITION_SHAPE ( 'NONE', 'NONE',  #23706 ) ;
#8006 = ORIENTED_EDGE ( 'NONE', *, *, #7466, .T. ) ;
#8007 = CARTESIAN_POINT ( 'NONE',  ( 4.999999999999999112, 9.241976615262160522, -1.699438267350405818 ) ) ;
#8008 = CIRCLE ( 'NONE', #1858, 4.000000000000001776 ) ;
#8009 = CARTESIAN_POINT ( 'NONE',  ( 55.59375000000000711, 11.65685424949236193, 10.99999999999998401 ) ) ;
#8010 = CARTESIAN_POINT ( 'NONE',  ( -1.647987302177966740E-14, -7.505553499465137612, -3.119443416399232394 ) ) ;
#8011 = DIRECTION ( 'NONE',  ( 0.06805114094563521898, -0.7054675904022857935, -0.7054675904022735811 ) ) ;
#8012 = CYLINDRICAL_SURFACE ( 'NONE', #7857, 8.265000000000021885 ) ;
#8013 = CARTESIAN_POINT ( 'NONE',  ( -11.83859044676619199, -9.000000000000003553, 5.000000000000079936 ) ) ;
#8014 = VERTEX_POINT ( 'NONE', #166 ) ;
#8015 = AXIS2_PLACEMENT_3D ( 'NONE', #19715, #12097, #14001 ) ;
#8016 = LINE ( 'NONE', #4404, #19882 ) ;
#8017 = ORIENTED_EDGE ( 'NONE', *, *, #20957, .F. ) ;
#8018 = FACE_OUTER_BOUND ( 'NONE', #16472, .T. ) ;
#8019 = DIRECTION ( 'NONE',  ( 0.000000000000000000, -1.224646799147353454E-16, 1.000000000000000000 ) ) ;
#8020 = VECTOR ( 'NONE', #11884, 1000.000000000000000 ) ;
#8021 = ORIENTED_EDGE ( 'NONE', *, *, #13604, .T. ) ;
#8022 = DIRECTION ( 'NONE',  ( -1.000000000000000000, -7.703719777548943412E-32, 0.000000000000000000 ) ) ;
#8023 = DIRECTION ( 'NONE',  ( 0.3420201433256622181, 0.9396926207859107594, -6.162975822039141593E-32 ) ) ;
#8024 = DIRECTION ( 'NONE',  ( 0.000000000000000000, 0.000000000000000000, 1.000000000000000000 ) ) ;
#8025 = CARTESIAN_POINT ( 'NONE',  ( -70.95000000218495018, 11.03553390593269867, 17.50000000000003908 ) ) ;
#8026 = EDGE_LOOP ( 'NONE', ( #6722, #17240, #13098 ) ) ;
#8027 = CARTESIAN_POINT ( 'NONE',  ( 4.000000000000000888, 4.898587196589412829E-16, 16.62500000273119838 ) ) ;
#8028 = EDGE_LOOP ( 'NONE', ( #21876, #344, #21715, #17173, #249 ) ) ;
#8029 = AXIS2_PLACEMENT_3D ( 'NONE', #8912, #7232, #21918 ) ;
#8030 = STYLED_ITEM ( 'NONE', ( #17564 ), #23619 ) ;
#8031 = CARTESIAN_POINT ( 'NONE',  ( 4.999999999999999112, 4.762163868918272591, 9.915734732513236338 ) ) ;
#8032 = STYLED_ITEM ( 'NONE', ( #2820 ), #21929 ) ;
#8033 = CARTESIAN_POINT ( 'NONE',  ( -3.999999999999998224, -1.656854249492383246, 15.06250000000001066 ) ) ;
#8034 = DIRECTION ( 'NONE',  ( -0.000000000000000000, -0.000000000000000000, -1.000000000000000000 ) ) ;
#8035 = EDGE_CURVE ( 'NONE', #4570, #21726, #13016, .T. ) ;
#8036 = EDGE_LOOP ( 'NONE', ( #20089, #23294, #13816, #7897 ) ) ;
#8037 = CARTESIAN_POINT ( 'NONE',  ( 3.250000000000004441, 5.629165124598849879, -3.700000000000000178 ) ) ;
#8038 = ADVANCED_FACE ( 'NONE', ( #3882 ), #11216, .F. ) ;
#8039 = DIRECTION ( 'NONE',  ( 1.000000000000000000, 0.000000000000000000, 0.000000000000000000 ) ) ;
#8040 = CARTESIAN_POINT ( 'NONE',  ( 71.75000000109247367, 8.538419263543524096, 13.53841926354352054 ) ) ;
#8041 = AXIS2_PLACEMENT_3D ( 'NONE', #14757, #5276, #16310 ) ;
#8042 = ORIENTED_EDGE ( 'NONE', *, *, #12319, .F. ) ;
#8043 = VECTOR ( 'NONE', #8110, 1000.000000000000000 ) ;
#8044 = CARTESIAN_POINT ( 'NONE',  ( 11.86036186966726191, -11.25000000000000355, 5.000000000000079936 ) ) ;
#8045 = CARTESIAN_POINT ( 'NONE',  ( 1.799999999999999600, 0.000000000000000000, 0.000000000000000000 ) ) ;
#8046 = EDGE_CURVE ( 'NONE', #13738, #12252, #280, .T. ) ;
#8047 = CARTESIAN_POINT ( 'NONE',  ( 70.45000000109247651, 12.06698730000000097, 14.99999999999999645 ) ) ;
#8048 = CARTESIAN_POINT ( 'NONE',  ( 2.445694354108821855, -2.445694354108820079, 14.81250000136560452 ) ) ;
#8049 = AXIS2_PLACEMENT_3D ( 'NONE', #19004, #19243, #8140 ) ;
#8050 = DIRECTION ( 'NONE',  ( 7.087422195345011518E-32, 1.000000000000000000, 0.000000000000000000 ) ) ;
#8051 = CARTESIAN_POINT ( 'NONE',  ( 0.000000000000000000, 0.000000000000000000, 0.000000000000000000 ) ) ;
#8052 = ORIENTED_EDGE ( 'NONE', *, *, #20012, .F. ) ;
#8053 = CARTESIAN_POINT ( 'NONE',  ( 2.828427124746189847, 2.828427124746190291, 0.9250000000000004885 ) ) ;
#8054 = DIRECTION ( 'NONE',  ( 1.000000000000000000, 0.000000000000000000, 0.000000000000000000 ) ) ;
#8055 = DIRECTION ( 'NONE',  ( 0.000000000000000000, 0.3090169943749411785, 0.9510565162951557516 ) ) ;
#8056 = CARTESIAN_POINT ( 'NONE',  ( 29.82104703033275328, -11.25000000000000355, 10.00000000000008882 ) ) ;
#8057 = EDGE_LOOP ( 'NONE', ( #916, #3703, #14720, #15636 ) ) ;
#8058 = CARTESIAN_POINT ( 'NONE',  ( -67.40000000109247935, 7.933012699999995476, 15.85617417291294196 ) ) ;
#8059 = ORIENTED_EDGE ( 'NONE', *, *, #14106, .T. ) ;
#8060 = CARTESIAN_POINT ( 'NONE',  ( 58.12500000000000000, 12.82842712474620228, 17.82842712474617386 ) ) ;
#8061 = CARTESIAN_POINT ( 'NONE',  ( -67.45000000109246230, 9.999999999999998224, 17.06698730000000097 ) ) ;
#8062 =( BOUNDED_CURVE ( )  B_SPLINE_CURVE ( 2, ( #3626, #14323, #8818, #3282, #21582, #23639, #19920, #19800, #18240 ),
 .UNSPECIFIED., .F., .F. ) 
 B_SPLINE_CURVE_WITH_KNOTS ( ( 3, 2, 2, 2, 3 ),
 ( 0.6250000000000005551, 0.6406250000000004441, 0.6562500000000003331, 0.6718750000000002220, 0.6875000000000001110 ),
 .UNSPECIFIED. ) 
 CURVE ( )  GEOMETRIC_REPRESENTATION_ITEM ( )  RATIONAL_B_SPLINE_CURVE ( ( 0.9999999999999973355, 0.9238795325112894030, 1.000000000000000000, 0.9238795325112867385, 1.000000000000000000, 0.9238795325112867385, 1.000000000000000000, 0.9238795325112861834, 1.000000000000000444 ) ) 
 REPRESENTATION_ITEM ( '' )  );
#8063 = ORIENTED_EDGE ( 'NONE', *, *, #5397, .F. ) ;
#8064 = CARTESIAN_POINT ( 'NONE',  ( 2.828427124746189847, 2.828427124746190291, -1.949999997268811791 ) ) ;
#8065 = VERTEX_POINT ( 'NONE', #3533 ) ;
#8066 = AXIS2_PLACEMENT_3D ( 'NONE', #12624, #7092, #18096 ) ;
#8067 = EDGE_CURVE ( 'NONE', #23046, #3718, #14479, .T. ) ;
#8068 = ORIENTED_EDGE ( 'NONE', *, *, #445, .F. ) ;
#8069 = CARTESIAN_POINT ( 'NONE',  ( 3.458734125000001658, 1.432654583217640498, 18.25000000136560629 ) ) ;
#8070 = CARTESIAN_POINT ( 'NONE',  ( 54.84375000000000000, 8.757359312880723223, 18.00000000000000355 ) ) ;
#8071 = VECTOR ( 'NONE', #9813, 1000.000000000000000 ) ;
#8072 = ADVANCED_FACE ( 'NONE', ( #20515 ), #2324, .T. ) ;
#8073 = CARTESIAN_POINT ( 'NONE',  ( -67.65000000109247935, 9.999999999999998224, 12.93301269999999192 ) ) ;
#8074 = VECTOR ( 'NONE', #16912, 1000.000000000000000 ) ;
#8075 = EDGE_CURVE ( 'NONE', #10540, #16693, #7211, .T. ) ;
#8076 = CARTESIAN_POINT ( 'NONE',  ( 69.90000000109247935, 7.933012699999995476, 14.14382582708705094 ) ) ;
#8077 = CARTESIAN_POINT ( 'NONE',  ( -66.60000000109246798, 10.85617417291294551, 17.06698729999999742 ) ) ;
#8078 = CARTESIAN_POINT ( 'NONE',  ( 4.999999999999999112, -9.241976615262169403, 1.699438267350339871 ) ) ;
#8079 = EDGE_CURVE ( 'NONE', #19075, #15133, #10284, .T. ) ;
#8080 = CARTESIAN_POINT ( 'NONE',  ( 57.15393183416157541, 6.971812294485357775, 16.17458954617365663 ) ) ;
#8081 = CARTESIAN_POINT ( 'NONE',  ( 0.000000000000000000, -9.241976615262146311, -1.699438267350473097 ) ) ;
#8082 = EDGE_CURVE ( 'NONE', #18634, #19718, #13338, .T. ) ;
#8083 = CARTESIAN_POINT ( 'NONE',  ( 6.353591512924457348E-16, -3.458734125000000770, 4.237500001365595459 ) ) ;
#8084 = DIRECTION ( 'NONE',  ( -1.000000000000000000, -0.000000000000000000, -0.000000000000000000 ) ) ;
#8085 = CARTESIAN_POINT ( 'NONE',  ( 2.828427124746192067, -2.828427124746189847, 12.50000000273119838 ) ) ;
#8086 = LINE ( 'NONE', #6154, #15345 ) ;
#8087 = CIRCLE ( 'NONE', #21426, 6.500000000000000888 ) ;
#8088 = EDGE_LOOP ( 'NONE', ( #11939, #14157, #18703, #4083 ) ) ;
#8089 = FACE_BOUND ( 'NONE', #9446, .T. ) ;
#8090 = ORIENTED_EDGE ( 'NONE', *, *, #1290, .F. ) ;
#8091 = CARTESIAN_POINT ( 'NONE',  ( 60.62268183416157541, 12.07320092032950676, 17.16943976678977180 ) ) ;
#8092 = CARTESIAN_POINT ( 'NONE',  ( 6.353591512924457348E-16, -3.458734125000000326, 0.9875000013655956810 ) ) ;
#8093 = CARTESIAN_POINT ( 'NONE',  ( 6.353591512924457348E-16, -3.458734125000000326, -1.012499998634402543 ) ) ;
#8094 = VERTEX_POINT ( 'NONE', #15524 ) ;
#8095 = CARTESIAN_POINT ( 'NONE',  ( -3.999999999999999112, 1.656854249492380804, 13.93750000000001243 ) ) ;
#8096 =( NAMED_UNIT ( * ) SI_UNIT ( $, .STERADIAN. ) SOLID_ANGLE_UNIT ( ) );
#8097 = FACE_OUTER_BOUND ( 'NONE', #2286, .T. ) ;
#8098 = ORIENTED_EDGE ( 'NONE', *, *, #1462, .T. ) ;
#8099 =( BOUNDED_SURFACE ( )  B_SPLINE_SURFACE ( 1, 2, ( 
 ( #6804, #21262, #14124, #21388, #4762, #21506, #5009, #8501, #21148, #15805, #19362, #1160, #5116, #10308, #12338, #3316, #13498, #1000, #18972, #15768, #22572, #19096, #11821, #15532, #20873, #9776, #882, #2688, #2443, #4366, #17434, #12056, #646, #775, #4612, #17197, #4481, #7980, #13729, #6413, #15652, #10029, #8333, #22679, #8108, #17316, #21108, #6535, #20992, #8217, #15418, #17073, #15299, #13853, #22800, #11947, #19212, #2800, #13963, #9903, #22923, #10143, #2554, #4723, #19322, #2911, #17552, #6178, #10259, #20759, #6292, #1117, #8462, #23039, #6650, #11703, #21222, #4837, #18857, #13609, #14886, #3840, #11408, #12968, #11049, #20346, #5762, #22019, #20230, #11537, #16544, #7450, #16658, #20588, #2390, #18807, #18335, #13320, #3953, #11287, #9367, #15121, #233, #14765, #2274, #18562, #14649, #3708, #18447, #9480, #13201, #2145, #1917, #20105, #7805, #5514, #16779, #22383, #5993, #9614, #4195, #9722, #17017, #13090, #22143, #120, #360, #7694, #15010 ),
 ( #11175, #9258, #593, #7566, #18685, #21906, #12848, #22265, #5635, #5877, #16904, #2027, #20467, #4073, #481, #4430, #22629, #8162, #13670, #17135, #11999, #11765, #20933, #8397, #13445, #22986, #17261, #19034, #17371, #2623, #4777, #711, #829, #8278, #19156, #10083, #8047, #13907, #18916, #939, #15593, #20707, #6115, #4665, #12114, #15362, #2972, #6591, #15714, #10324, #15473, #4549, #21165, #1059, #19265, #19376, #17614, #7918, #6356, #22743, #6232, #11885, #2743, #22861, #9967, #22505, #6475, #2505, #13553, #9839, #15238, #13796, #2853, #4312, #11650, #21053, #20820, #10203, #17491, #4901, #16286, #3334, #3102, #21405, #15929, #1402, #6948, #10444, #5250, #5023, #14263, #1652, #6703, #23579, #10560, #12353, #10678, #19615, #21767, #17724, #17835, #1533, #12471, #17953, #1287, #7187, #12237, #8875, #16169, #14017, #23092, #21644, #5376, #8625, #19969, #14502, #8996, #3571, #8744, #12597, #3213, #23455, #8517, #12717, #10907, #14140, #23205, #5134, #7063 ) ),
 .UNSPECIFIED., .F., .F., .F. ) 
 B_SPLINE_SURFACE_WITH_KNOTS ( ( 2, 2 ),
 ( 3, 2, 2, 2, 2, 2, 2, 2, 2, 2, 2, 2, 2, 2, 2, 2, 2, 2, 2, 2, 2, 2, 2, 2, 2, 2, 2, 2, 2, 2, 2, 2, 2, 2, 2, 2, 2, 2, 2, 2, 2, 2, 2, 2, 2, 2, 2, 2, 2, 2, 2, 2, 2, 2, 2, 2, 2, 2, 2, 2, 2, 2, 2, 2, 3 ),
 ( 0.000000000000000000, 1.000000000000000000 ),
 ( 0.000000000000000000, 0.01562500000000000000, 0.03125000000000000000, 0.04687500000000000000, 0.06250000000000000000, 0.07812500000000000000, 0.09375000000000000000, 0.1093750000000000000, 0.1250000000000000000, 0.1406250000000000000, 0.1562500000000000000, 0.1718750000000000000, 0.1875000000000000000, 0.2031250000000000000, 0.2187500000000000000, 0.2343750000000000000, 0.2500000000000000000, 0.2656250000000000000, 0.2812500000000000000, 0.2968750000000000000, 0.3125000000000000000, 0.3281250000000000000, 0.3437500000000000000, 0.3593750000000000000, 0.3750000000000000000, 0.3906250000000000000, 0.4062500000000000000, 0.4218750000000000000, 0.4375000000000000000, 0.4531250000000000000, 0.4687500000000000000, 0.4843750000000000000, 0.5000000000000000000, 0.5156250000000000000, 0.5312500000000000000, 0.5468750000000000000, 0.5625000000000000000, 0.5781250000000000000, 0.5937500000000000000, 0.6093750000000000000, 0.6250000000000000000, 0.6406250000000000000, 0.6562500000000000000, 0.6718750000000000000, 0.6875000000000000000, 0.7031250000000000000, 0.7187500000000000000, 0.7343750000000000000, 0.7500000000000000000, 0.7656250000000000000, 0.7812500000000000000, 0.7968750000000000000, 0.8125000000000000000, 0.8281250000000000000, 0.8437500000000000000, 0.8593750000000000000, 0.8750000000000000000, 0.8906250000000000000, 0.9062500000000000000, 0.9218750000000000000, 0.9375000000000000000, 0.9531250000000000000, 0.9687500000000000000, 0.9843750000000000000, 1.000000000000000000 ),
 .UNSPECIFIED. ) 
 GEOMETRIC_REPRESENTATION_ITEM ( )  RATIONAL_B_SPLINE_SURFACE ( (
 ( 1.000000000000000000, 0.9238795325112867385, 1.000000000000000000, 0.9238795325112867385, 1.000000000000000000, 0.9238795325112867385, 1.000000000000000000, 0.9238795325112867385, 1.000000000000000000, 0.9238795325112867385, 1.000000000000000000, 0.9238795325112867385, 1.000000000000000000, 0.9238795325112867385, 1.000000000000000000, 0.9238795325112867385, 1.000000000000000000, 0.9238795325112867385, 1.000000000000000000, 0.9238795325112867385, 1.000000000000000000, 0.9238795325112867385, 1.000000000000000000, 0.9238795325112867385, 1.000000000000000000, 0.9238795325112867385, 1.000000000000000000, 0.9238795325112867385, 1.000000000000000000, 0.9238795325112867385, 1.000000000000000000, 0.9238795325112867385, 1.000000000000000000, 0.9238795325112867385, 1.000000000000000000, 0.9238795325112867385, 1.000000000000000000, 0.9238795325112867385, 1.000000000000000000, 0.9238795325112867385, 1.000000000000000000, 0.9238795325112867385, 1.000000000000000000, 0.9238795325112867385, 1.000000000000000000, 0.9238795325112867385, 1.000000000000000000, 0.9238795325112867385, 1.000000000000000000, 0.9238795325112867385, 1.000000000000000000, 0.9238795325112867385, 1.000000000000000000, 0.9238795325112867385, 1.000000000000000000, 0.9238795325112867385, 1.000000000000000000, 0.9238795325112867385, 1.000000000000000000, 0.9238795325112867385, 1.000000000000000000, 0.9238795325112867385, 1.000000000000000000, 0.9238795325112867385, 1.000000000000000000, 0.9238795325112867385, 1.000000000000000000, 0.9238795325112867385, 1.000000000000000000, 0.9238795325112867385, 1.000000000000000000, 0.9238795325112867385, 1.000000000000000000, 0.9238795325112867385, 1.000000000000000000, 0.9238795325112867385, 1.000000000000000000, 0.9238795325112867385, 1.000000000000000000, 0.9238795325112867385, 1.000000000000000000, 0.9238795325112867385, 1.000000000000000000, 0.9238795325112867385, 1.000000000000000000, 0.9238795325112867385, 1.000000000000000000, 0.9238795325112867385, 1.000000000000000000, 0.9238795325112867385, 1.000000000000000000, 0.9238795325112867385, 1.000000000000000000, 0.9238795325112867385, 1.000000000000000000, 0.9238795325112867385, 1.000000000000000000, 0.9238795325112867385, 1.000000000000000000, 0.9238795325112867385, 1.000000000000000000, 0.9238795325112867385, 1.000000000000000000, 0.9238795325112867385, 1.000000000000000000, 0.9238795325112867385, 1.000000000000000000, 0.9238795325112867385, 1.000000000000000000, 0.9238795325112867385, 1.000000000000000000, 0.9238795325112867385, 1.000000000000000000, 0.9238795325112867385, 1.000000000000000000, 0.9238795325112867385, 1.000000000000000000, 0.9238795325112867385, 1.000000000000000000, 0.9238795325112867385, 1.000000000000000000, 0.9238795325112867385, 1.000000000000000000, 0.9238795325112867385, 1.000000000000000000, 0.9238795325112867385, 1.000000000000000000, 0.9238795325112867385, 1.000000000000000000),
 ( 1.000000000000000000, 0.9238795325112867385, 1.000000000000000000, 0.9238795325112867385, 1.000000000000000000, 0.9238795325112867385, 1.000000000000000000, 0.9238795325112867385, 1.000000000000000000, 0.9238795325112867385, 1.000000000000000000, 0.9238795325112867385, 1.000000000000000000, 0.9238795325112867385, 1.000000000000000000, 0.9238795325112867385, 1.000000000000000000, 0.9238795325112867385, 1.000000000000000000, 0.9238795325112867385, 1.000000000000000000, 0.9238795325112867385, 1.000000000000000000, 0.9238795325112867385, 1.000000000000000000, 0.9238795325112867385, 1.000000000000000000, 0.9238795325112867385, 1.000000000000000000, 0.9238795325112867385, 1.000000000000000000, 0.9238795325112867385, 1.000000000000000000, 0.9238795325112867385, 1.000000000000000000, 0.9238795325112867385, 1.000000000000000000, 0.9238795325112867385, 1.000000000000000000, 0.9238795325112867385, 1.000000000000000000, 0.9238795325112867385, 1.000000000000000000, 0.9238795325112867385, 1.000000000000000000, 0.9238795325112867385, 1.000000000000000000, 0.9238795325112867385, 1.000000000000000000, 0.9238795325112867385, 1.000000000000000000, 0.9238795325112867385, 1.000000000000000000, 0.9238795325112867385, 1.000000000000000000, 0.9238795325112867385, 1.000000000000000000, 0.9238795325112867385, 1.000000000000000000, 0.9238795325112867385, 1.000000000000000000, 0.9238795325112867385, 1.000000000000000000, 0.9238795325112867385, 1.000000000000000000, 0.9238795325112867385, 1.000000000000000000, 0.9238795325112867385, 1.000000000000000000, 0.9238795325112867385, 1.000000000000000000, 0.9238795325112867385, 1.000000000000000000, 0.9238795325112867385, 1.000000000000000000, 0.9238795325112867385, 1.000000000000000000, 0.9238795325112867385, 1.000000000000000000, 0.9238795325112867385, 1.000000000000000000, 0.9238795325112867385, 1.000000000000000000, 0.9238795325112867385, 1.000000000000000000, 0.9238795325112867385, 1.000000000000000000, 0.9238795325112867385, 1.000000000000000000, 0.9238795325112867385, 1.000000000000000000, 0.9238795325112867385, 1.000000000000000000, 0.9238795325112867385, 1.000000000000000000, 0.9238795325112867385, 1.000000000000000000, 0.9238795325112867385, 1.000000000000000000, 0.9238795325112867385, 1.000000000000000000, 0.9238795325112867385, 1.000000000000000000, 0.9238795325112867385, 1.000000000000000000, 0.9238795325112867385, 1.000000000000000000, 0.9238795325112867385, 1.000000000000000000, 0.9238795325112867385, 1.000000000000000000, 0.9238795325112867385, 1.000000000000000000, 0.9238795325112867385, 1.000000000000000000, 0.9238795325112867385, 1.000000000000000000, 0.9238795325112867385, 1.000000000000000000, 0.9238795325112867385, 1.000000000000000000, 0.9238795325112867385, 1.000000000000000000, 0.9238795325112867385, 1.000000000000000000, 0.9238795325112867385, 1.000000000000000000, 0.9238795325112867385, 1.000000000000000000) ) ) 
 REPRESENTATION_ITEM ( '' )  SURFACE ( )  );
#8100 = CARTESIAN_POINT ( 'NONE',  ( -69.10000000218495586, 11.76776695296636888, 13.23223304703362579 ) ) ;
#8101 = EDGE_CURVE ( 'NONE', #17388, #5511, #5806, .T. ) ;
#8102 = CARTESIAN_POINT ( 'NONE',  ( 2.445694354108820967, -2.445694354108820079, -2.637499998634404097 ) ) ;
#8103 = AXIS2_PLACEMENT_3D ( 'NONE', #4905, #12719, #1407 ) ;
#8104 = CARTESIAN_POINT ( 'NONE',  ( -3.250000000000004885, -5.629165124598848990, -3.700000000000000178 ) ) ;
#8105 = ADVANCED_FACE ( 'NONE', ( #8097 ), #526, .F. ) ;
#8106 = DIRECTION ( 'NONE',  ( 1.000000000000000000, 0.000000000000000000, 0.000000000000000000 ) ) ;
#8107 = CARTESIAN_POINT ( 'NONE',  ( -3.999999999999999112, 0.000000000000000000, 11.00000000000001066 ) ) ;
#8108 = CARTESIAN_POINT ( 'NONE',  ( 69.85000000109248219, 7.933012699999995476, 14.99999999999999645 ) ) ;
#8109 = EDGE_CURVE ( 'NONE', #22760, #2984, #4897, .T. ) ;
#8110 = DIRECTION ( 'NONE',  ( -1.000000000000000000, -7.703719777548943412E-32, 0.000000000000000000 ) ) ;
#8111 = CARTESIAN_POINT ( 'NONE',  ( 56.37731816583843170, 7.830560233210212218, 12.92679907967049679 ) ) ;
#8112 = CARTESIAN_POINT ( 'NONE',  ( -3.458734125000000326, 0.000000000000000000, -2.262499998634403653 ) ) ;
#8113 = CARTESIAN_POINT ( 'NONE',  ( -1.432654583217639832, -3.458734125000000326, 12.87500000136560629 ) ) ;
#8114 = CARTESIAN_POINT ( 'NONE',  ( 21.00000000000000355, 2.516649172247811061E-16, -2.055000000000000160 ) ) ;
#8115 = CARTESIAN_POINT ( 'NONE',  ( -68.80000000109247082, 12.06698729999999919, 14.14382582708705094 ) ) ;
#8116 = LINE ( 'NONE', #15660, #2021 ) ;
#8117 = DIRECTION ( 'NONE',  ( -1.000000000000000000, 0.000000000000000000, 1.982541115402065110E-16 ) ) ;
#8118 = ORIENTED_EDGE ( 'NONE', *, *, #14745, .F. ) ;
#8119 = CARTESIAN_POINT ( 'NONE',  ( 4.000000000000000888, 4.898587196589412829E-16, 14.50000000000001066 ) ) ;
#8120 = DIRECTION ( 'NONE',  ( 0.3420201433256622181, -0.9396926207859107594, 0.000000000000000000 ) ) ;
#8121 = CARTESIAN_POINT ( 'NONE',  ( -69.80000000109247082, 7.933012699999995476, 15.85617417291294196 ) ) ;
#8122 = ORIENTED_EDGE ( 'NONE', *, *, #5286, .T. ) ;
#8123 = ORIENTED_EDGE ( 'NONE', *, *, #20956, .T. ) ;
#8124 = DIRECTION ( 'NONE',  ( -1.000000000000000000, -0.000000000000000000, -0.000000000000000000 ) ) ;
#8125 = PLANE ( 'NONE',  #11802 ) ;
#8126 = ORIENTED_EDGE ( 'NONE', *, *, #14272, .F. ) ;
#8127 = CARTESIAN_POINT ( 'NONE',  ( 0.5469614295415388128, -4.303013824935362663, -3.535263753543555598 ) ) ;
#8128 = UNCERTAINTY_MEASURE_WITH_UNIT (LENGTH_MEASURE( 1.000000000000000082E-05 ), #8580, 'distance_accuracy_value', 'NONE');
#8129 = CARTESIAN_POINT ( 'NONE',  ( 68.40000000109249356, 9.143825827087050939, 12.93301269999999370 ) ) ;
#8130 = CARTESIAN_POINT ( 'NONE',  ( 67.70000000109246230, 7.933012699999995476, 14.14382582708705094 ) ) ;
#8131 = EDGE_CURVE ( 'NONE', #10478, #7307, #13133, .T. ) ;
#8132 = ORIENTED_EDGE ( 'NONE', *, *, #14577, .T. ) ;
#8133 = DIRECTION ( 'NONE',  ( -1.000000000000000000, 0.000000000000000000, 0.000000000000000000 ) ) ;
#8134 = CARTESIAN_POINT ( 'NONE',  ( 55.21875000000000000, 14.00000000000000888, 16.65685424949235482 ) ) ;
#8135 = CARTESIAN_POINT ( 'NONE',  ( 71.50000000218496155, 11.76776695296636888, 13.23223304703362579 ) ) ;
#8136 = CARTESIAN_POINT ( 'NONE',  ( 3.458734125000001214, 1.432654583217640498, 18.00000000136560274 ) ) ;
#8137 = DIRECTION ( 'NONE',  ( -1.000000000000000000, 0.000000000000000000, 0.000000000000000000 ) ) ;
#8138 = FACE_OUTER_BOUND ( 'NONE', #22549, .T. ) ;
#8139 = VERTEX_POINT ( 'NONE', #4472 ) ;
#8140 = DIRECTION ( 'NONE',  ( -1.000000000000000000, 0.000000000000000000, 0.000000000000000000 ) ) ;
#8141 = DIRECTION ( 'NONE',  ( -7.087422195345011518E-32, -1.000000000000000000, -0.000000000000000000 ) ) ;
#8142 = CARTESIAN_POINT ( 'NONE',  ( -19.99999999999999645, -9.000000000000003553, 10.00000000000008882 ) ) ;
#8143 = ORIENTED_EDGE ( 'NONE', *, *, #21164, .F. ) ;
#8144 = CARTESIAN_POINT ( 'NONE',  ( -19.99999999999999645, -9.000000000000003553, 10.00000000000008882 ) ) ;
#8145 = CARTESIAN_POINT ( 'NONE',  ( -27.50000000000000711, 7.500000000000002665, -33.66025403784446723 ) ) ;
#8146 = CARTESIAN_POINT ( 'NONE',  ( -1.656854249492380138, -3.999999999999999112, 11.31250000273119660 ) ) ;
#8147 = AXIS2_PLACEMENT_3D ( 'NONE', #810, #22720, #20800 ) ;
#8148 = PLANE ( 'NONE',  #9501 ) ;
#8149 = EDGE_LOOP ( 'NONE', ( #5532, #9435, #17962, #13430 ) ) ;
#8150 = CARTESIAN_POINT ( 'NONE',  ( 2.828427124746189847, 2.828427124746190291, 0.9250000000000004885 ) ) ;
#8151 = ORIENTED_EDGE ( 'NONE', *, *, #16575, .F. ) ;
#8152 = CARTESIAN_POINT ( 'NONE',  ( -19.99999999999999645, -11.25000000000000355, 5.000000000000079936 ) ) ;
#8153 = CARTESIAN_POINT ( 'NONE',  ( -1.656854249492380138, -3.999999999999999112, 11.18750000000000888 ) ) ;
#8154 = CARTESIAN_POINT ( 'NONE',  ( 71.55000000218494449, 12.50000000000000000, 13.96446609406725869 ) ) ;
#8155 = ORIENTED_EDGE ( 'NONE', *, *, #11296, .T. ) ;
#8156 = DIRECTION ( 'NONE',  ( 0.000000000000000000, 0.000000000000000000, 1.000000000000000000 ) ) ;
#8157 = CARTESIAN_POINT ( 'NONE',  ( 7.829898480332751376, -11.25000000000000355, 5.000000000000079936 ) ) ;
#8158 = CARTESIAN_POINT ( 'NONE',  ( 66.95000000109246230, 8.538419263543524096, 13.53841926354352054 ) ) ;
#8159 = EDGE_LOOP ( 'NONE', ( #21858, #14543, #9266, #17145 ) ) ;
#8160 = CARTESIAN_POINT ( 'NONE',  ( 3.250000000000003109, 5.629165124598848102, 1.734723475976807094E-15 ) ) ;
#8161 = CARTESIAN_POINT ( 'NONE',  ( -4.211140560182196957, -2.431303136016552013, -3.745885042887436178 ) ) ;
#8162 = CARTESIAN_POINT ( 'NONE',  ( 71.40000000109246514, 10.85617417291294551, 17.06698729999999742 ) ) ;
#8163 = CARTESIAN_POINT ( 'NONE',  ( 3.458734125000001214, 4.235727675282971730E-16, 13.93750000136560629 ) ) ;
#8164 = CARTESIAN_POINT ( 'NONE',  ( 40.13469571966727045, -11.25000000000000355, 5.000000000000079936 ) ) ;
#8165 = ORIENTED_EDGE ( 'NONE', *, *, #11151, .T. ) ;
#8166 = CARTESIAN_POINT ( 'NONE',  ( -2.828427124746189403, -2.828427124746190735, 0.4250000000000017653 ) ) ;
#8167 = DIRECTION ( 'NONE',  ( -1.000000000000000000, -0.000000000000000000, 0.000000000000000000 ) ) ;
#8168 = CARTESIAN_POINT ( 'NONE',  ( 1.432654583217643163, -3.458734124999999437, 10.75000000136560452 ) ) ;
#8169 = DIRECTION ( 'NONE',  ( 1.000000000000000000, 0.000000000000000000, 0.000000000000000000 ) ) ;
#8170 = EDGE_LOOP ( 'NONE', ( #5027, #11985, #19894, #15942 ) ) ;
#8171 = EDGE_CURVE ( 'NONE', #19202, #8553, #9657, .T. ) ;
#8172 = CARTESIAN_POINT ( 'NONE',  ( -67.30000000109247082, 9.143825827087049163, 17.06698730000000097 ) ) ;
#8173 = EDGE_LOOP ( 'NONE', ( #22009, #12284, #356, #3382 ) ) ;
#8174 = CARTESIAN_POINT ( 'NONE',  ( -67.20000000109247651, 12.06698730000000275, 14.14382582708705094 ) ) ;
#8175 = ORIENTED_EDGE ( 'NONE', *, *, #1966, .T. ) ;
#8176 = FACE_OUTER_BOUND ( 'NONE', #22663, .T. ) ;
#8177 = ORIENTED_EDGE ( 'NONE', *, *, #12594, .T. ) ;
#8178 = ORIENTED_EDGE ( 'NONE', *, *, #11158, .T. ) ;
#8179 = CARTESIAN_POINT ( 'NONE',  ( 2.445694354108822299, -2.445694354108820079, 13.06250000136560629 ) ) ;
#8180 = EDGE_CURVE ( 'NONE', #5464, #14452, #11461, .T. ) ;
#8181 = CARTESIAN_POINT ( 'NONE',  ( -14.99999999999996980, -15.00000000000000000, -19.99999999999999645 ) ) ;
#8182 = CIRCLE ( 'NONE', #16210, 8.749000000000000554 ) ;
#8183 = CARTESIAN_POINT ( 'NONE',  ( -67.85000000109248219, 12.06698730000000097, 14.99999999999999645 ) ) ;
#8184 = VECTOR ( 'NONE', #17268, 1000.000000000000000 ) ;
#8185 = CARTESIAN_POINT ( 'NONE',  ( 70.30000000109247082, 12.06698729999999919, 15.85617417291294196 ) ) ;
#8186 = CARTESIAN_POINT ( 'NONE',  ( -66.05000000109247082, 7.933012699999995476, 14.99999999999999645 ) ) ;
#8187 = CARTESIAN_POINT ( 'NONE',  ( 7.001720609283449193, -8.974600000000002353, 5.000000000000079936 ) ) ;
#8188 = CARTESIAN_POINT ( 'NONE',  ( 54.81018183416157541, 12.99999999999999822, 15.06805114094562192 ) ) ;
#8189 = DIRECTION ( 'NONE',  ( 0.000000000000000000, 0.000000000000000000, -1.000000000000000000 ) ) ;
#8190 =( BOUNDED_CURVE ( )  B_SPLINE_CURVE ( 2, ( #11852, #20556, #15331, #19128, #15567, #17345, #6205, #13639, #4397 ),
 .UNSPECIFIED., .F., .F. ) 
 B_SPLINE_CURVE_WITH_KNOTS ( ( 3, 2, 2, 2, 3 ),
 ( 0.6500000000000000222, 0.6624999999999999778, 0.6750000000000000444, 0.6875000000000000000, 0.6999999999999999556 ),
 .UNSPECIFIED. ) 
 CURVE ( )  GEOMETRIC_REPRESENTATION_ITEM ( )  RATIONAL_B_SPLINE_CURVE ( ( 1.000000000000000000, 0.9238795325112867385, 1.000000000000000000, 0.9238795325112867385, 1.000000000000000000, 0.9238795325112867385, 1.000000000000000000, 0.9238795325112867385, 1.000000000000000000 ) ) 
 REPRESENTATION_ITEM ( '' )  );
#8191 = CARTESIAN_POINT ( 'NONE',  ( -3.458734125000000326, -1.432654583217642497, 2.050000001365597679 ) ) ;
#8192 = CARTESIAN_POINT ( 'NONE',  ( 0.000000000000000000, 0.000000000000000000, 0.000000000000000000 ) ) ;
#8193 = CARTESIAN_POINT ( 'NONE',  ( -1.656854249492379250, 4.000000000000000000, 10.93750000273119483 ) ) ;
#8194 = CARTESIAN_POINT ( 'NONE',  ( 60.00000000000000711, 15.00000000000000000, 24.99999999999999645 ) ) ;
#8195 = EDGE_LOOP ( 'NONE', ( #8307, #7299, #3217, #11695 ) ) ;
#8196 = EDGE_CURVE ( 'NONE', #23499, #10094, #4356, .T. ) ;
#8197 = LINE ( 'NONE', #2666, #7471 ) ;
#8198 = ORIENTED_EDGE ( 'NONE', *, *, #11437, .F. ) ;
#8199 = CARTESIAN_POINT ( 'NONE',  ( 59.59143183416158962, 11.31069182806491291, 12.02818770551463778 ) ) ;
#8200 = CARTESIAN_POINT ( 'NONE',  ( 2.445694354108820523, -2.445694354108820079, 0.1125000013655966247 ) ) ;
#8201 = EDGE_CURVE ( 'NONE', #7525, #3785, #9535, .T. ) ;
#8202 = ORIENTED_EDGE ( 'NONE', *, *, #17689, .F. ) ;
#8203 = LINE ( 'NONE', #12282, #15646 ) ;
#8204 = DIRECTION ( 'NONE',  ( 0.000000000000000000, 0.000000000000000000, 1.000000000000000000 ) ) ;
#8205 = ORIENTED_EDGE ( 'NONE', *, *, #5101, .T. ) ;
#8206 = DIRECTION ( 'NONE',  ( 0.000000000000000000, 0.000000000000000000, -1.000000000000000000 ) ) ;
#8207 = ORIENTED_EDGE ( 'NONE', *, *, #15076, .T. ) ;
#8208 = EDGE_CURVE ( 'NONE', #8531, #10374, #19634, .T. ) ;
#8209 = CARTESIAN_POINT ( 'NONE',  ( 56.93981816583843170, 10.06805114094563791, 17.99999999999999645 ) ) ;
#8210 = EDGE_CURVE ( 'NONE', #8667, #13749, #7970, .T. ) ;
#8211 = CONICAL_SURFACE ( 'NONE', #143, 6.500000000000000888, 1.047197551196596521 ) ;
#8212 = CARTESIAN_POINT ( 'NONE',  ( -70.50000000218494733, 8.232233047033629347, 13.23223304703362402 ) ) ;
#8213 = DIRECTION ( 'NONE',  ( -1.000000000000000000, 0.000000000000000000, 0.000000000000000000 ) ) ;
#8214 = CARTESIAN_POINT ( 'NONE',  ( -4.154094228333736538, -2.398367420967545627, -3.721909803043222276 ) ) ;
#8215 = FACE_OUTER_BOUND ( 'NONE', #1609, .T. ) ;
#8216 = CARTESIAN_POINT ( 'NONE',  ( 45.00000000000000000, -2.399706452296379577, 55.00000000000021316 ) ) ;
#8217 = CARTESIAN_POINT ( 'NONE',  ( 69.60000000109249640, 10.85617417291294551, 17.06698729999999742 ) ) ;
#8218 = FACE_OUTER_BOUND ( 'NONE', #6068, .T. ) ;
#8219 = CARTESIAN_POINT ( 'NONE',  ( 57.22106816583844591, 13.02818770551464489, 16.17458954617363531 ) ) ;
#8220 = EDGE_CURVE ( 'NONE', #19365, #11955, #8739, .T. ) ;
#8221 = CARTESIAN_POINT ( 'NONE',  ( -3.458734125000000770, 0.000000000000000000, 4.987500001365595459 ) ) ;
#8222 = CARTESIAN_POINT ( 'NONE',  ( 2.445694354108821411, 2.445694354108820523, 11.31250000136560452 ) ) ;
#8223 =( NAMED_UNIT ( * ) PLANE_ANGLE_UNIT ( ) SI_UNIT ( $, .RADIAN. ) );
#8224 = CARTESIAN_POINT ( 'NONE',  ( -69.05000000109247082, 9.999999999999998224, 17.06698730000000097 ) ) ;
#8225 = LINE ( 'NONE', #8471, #11242 ) ;
#8226 = CARTESIAN_POINT ( 'NONE',  ( 4.999999999999999112, 6.478011392632982535, -6.807171995660517005 ) ) ;
#8227 = EDGE_LOOP ( 'NONE', ( #20489, #17327, #22883, #5778 ) ) ;
#8228 = DIRECTION ( 'NONE',  ( 0.000000000000000000, 0.000000000000000000, 1.000000000000000000 ) ) ;
#8229 = AXIS2_PLACEMENT_3D ( 'NONE', #10039, #17326, #891 ) ;
#8230 = CARTESIAN_POINT ( 'NONE',  ( 4.000000000000000000, 4.898587196589412829E-16, 2.925000002731188875 ) ) ;
#8231 = EDGE_CURVE ( 'NONE', #6195, #14695, #766, .T. ) ;
#8232 = AXIS2_PLACEMENT_3D ( 'NONE', #22745, #4432, #9616 ) ;
#8233 = ORIENTED_EDGE ( 'NONE', *, *, #22573, .F. ) ;
#8234 = ORIENTED_EDGE ( 'NONE', *, *, #20443, .F. ) ;
#8235 = LINE ( 'NONE', #13513, #3335 ) ;
#8236 = CARTESIAN_POINT ( 'NONE',  ( 20.55500000000001748, 0.000000000000000000, 2.500000000000000888 ) ) ;
#8237 = ORIENTED_EDGE ( 'NONE', *, *, #20338, .T. ) ;
#8238 = EDGE_CURVE ( 'NONE', #990, #11486, #4518, .T. ) ;
#8239 = CARTESIAN_POINT ( 'NONE',  ( 1.257172072275274388, -3.892973519170983110, -3.433252694550781303 ) ) ;
#8240 = EDGE_CURVE ( 'NONE', #16346, #19924, #7595, .T. ) ;
#8241 = CARTESIAN_POINT ( 'NONE',  ( 69.70000000109246230, 9.143825827087049163, 17.06698729999999742 ) ) ;
#8242 = VECTOR ( 'NONE', #5389, 1000.000000000000000 ) ;
#8243 = CARTESIAN_POINT ( 'NONE',  ( 68.95000000109247651, 11.46158073645647235, 16.46158073645647235 ) ) ;
#8244 = CIRCLE ( 'NONE', #178, 6.200000000000020606 ) ;
#8245 = EDGE_LOOP ( 'NONE', ( #18912, #1902, #18824, #17481 ) ) ;
#8246 = CARTESIAN_POINT ( 'NONE',  ( -60.00000000000000711, 15.00000000000000000, 10.00000000000008882 ) ) ;
#8247 = CARTESIAN_POINT ( 'NONE',  ( 54.18750000000000711, 9.999999999999978684, 10.99999999999999645 ) ) ;
#8248 = CARTESIAN_POINT ( 'NONE',  ( 55.00000000000000711, -9.999999999999998224, 19.99999999999999645 ) ) ;
#8249 = CARTESIAN_POINT ( 'NONE',  ( 4.999999999999999112, 0.4999240074895661690, -8.734705317681621395 ) ) ;
#8250 = CARTESIAN_POINT ( 'NONE',  ( 1.506022603841296714, 0.000000000000000000, 0.000000000000000000 ) ) ;
#8251 = DIRECTION ( 'NONE',  ( -0.000000000000000000, -0.000000000000000000, 1.000000000000000000 ) ) ;
#8252 = ORIENTED_EDGE ( 'NONE', *, *, #7005, .F. ) ;
#8253 = DIRECTION ( 'NONE',  ( 0.000000000000000000, 0.000000000000000000, -1.000000000000000000 ) ) ;
#8254 = DIRECTION ( 'NONE',  ( -1.000000000000000000, -0.000000000000000000, -0.000000000000000000 ) ) ;
#8255 = LINE ( 'NONE', #919, #10452 ) ;
#8256 = VERTEX_POINT ( 'NONE', #8675 ) ;
#8257 = CARTESIAN_POINT ( 'NONE',  ( -4.000000000000000000, 0.000000000000000000, -1.699999999999998401 ) ) ;
#8258 = DIRECTION ( 'NONE',  ( 0.9396926207859107594, -0.3420201433256623291, 3.697785493223492838E-32 ) ) ;
#8259 = DIRECTION ( 'NONE',  ( -1.000000000000000000, -0.000000000000000000, -0.000000000000000000 ) ) ;
#8260 = VECTOR ( 'NONE', #12984, 1000.000000000000000 ) ;
#8261 = EDGE_CURVE ( 'NONE', #4946, #22848, #8369, .T. ) ;
#8262 = CARTESIAN_POINT ( 'NONE',  ( -9.311853653233800543, -9.000000000000005329, 5.000000000000079936 ) ) ;
#8263 = ORIENTED_EDGE ( 'NONE', *, *, #12761, .F. ) ;
#8264 = CARTESIAN_POINT ( 'NONE',  ( 72.50000000000000000, 9.999999999999998224, 17.49999999999999645 ) ) ;
#8265 = EDGE_LOOP ( 'NONE', ( #17214, #12442, #12273, #7073 ) ) ;
#8266 = ADVANCED_FACE ( 'NONE', ( #15975 ), #10611, .F. ) ;
#8267 = CARTESIAN_POINT ( 'NONE',  ( 71.75000000109248788, 11.46158073645647235, 13.53841926354352232 ) ) ;
#8268 = CARTESIAN_POINT ( 'NONE',  ( 70.45000000218493597, 7.499999999999995559, 13.96446609406725692 ) ) ;
#8269 = AXIS2_PLACEMENT_3D ( 'NONE', #11033, #3821, #16889 ) ;
#8270 = AXIS2_PLACEMENT_3D ( 'NONE', #13647, #8254, #4757 ) ;
#8271 = DIRECTION ( 'NONE',  ( -1.000000000000000000, 0.000000000000000000, 0.000000000000000000 ) ) ;
#8272 = DIRECTION ( 'NONE',  ( 0.000000000000000000, -0.9510565162951565288, 0.3090169943749382364 ) ) ;
#8273 = CARTESIAN_POINT ( 'NONE',  ( 66.60000000109246798, 10.85617417291294551, 17.06698730000000097 ) ) ;
#8274 = ORIENTED_EDGE ( 'NONE', *, *, #17745, .T. ) ;
#8275 = VECTOR ( 'NONE', #13461, 999.9999999999998863 ) ;
#8276 = CARTESIAN_POINT ( 'NONE',  ( -4.898587196589412829E-16, 0.000000000000000000, -4.000000000000000000 ) ) ;
#8277 = CARTESIAN_POINT ( 'NONE',  ( -65.00000000000000000, -10.00000000000000178, 14.99999999999999467 ) ) ;
#8278 = CARTESIAN_POINT ( 'NONE',  ( 70.60000000109246798, 10.85617417291294551, 17.06698729999999742 ) ) ;
#8279 = CARTESIAN_POINT ( 'NONE',  ( -1.432654583217639610, -3.458734124999999882, 13.62500000136560452 ) ) ;
#8280 = DIRECTION ( 'NONE',  ( 0.000000000000000000, 0.5877852522924684742, 0.8090169943749507819 ) ) ;
#8281 = DIRECTION ( 'NONE',  ( -1.000000000000000000, -0.000000000000000000, -0.000000000000000000 ) ) ;
#8282 = ORIENTED_EDGE ( 'NONE', *, *, #15707, .F. ) ;
#8283 = CARTESIAN_POINT ( 'NONE',  ( -1.656854249492380804, 4.000000000000000000, -1.887499999999998179 ) ) ;
#8284 = DIRECTION ( 'NONE',  ( 0.000000000000000000, 0.000000000000000000, 1.000000000000000000 ) ) ;
#8285 = DIRECTION ( 'NONE',  ( -1.000000000000000000, 0.000000000000000000, 0.000000000000000000 ) ) ;
#8286 = DIRECTION ( 'NONE',  ( -1.000000000000000000, -7.703719777548943412E-32, 0.000000000000000000 ) ) ;
#8287 = ORIENTED_EDGE ( 'NONE', *, *, #3331, .T. ) ;
#8288 = ORIENTED_EDGE ( 'NONE', *, *, #11437, .T. ) ;
#8289 = CARTESIAN_POINT ( 'NONE',  ( -67.65000000109247935, 7.933012699999995476, 14.99999999999999645 ) ) ;
#8290 = ORIENTED_EDGE ( 'NONE', *, *, #1029, .T. ) ;
#8291 = DIRECTION ( 'NONE',  ( 0.3420201433256622181, 0.9396926207859107594, -6.162975822039141593E-32 ) ) ;
#8292 = EDGE_LOOP ( 'NONE', ( #4511, #22396, #11863, #7893 ) ) ;
#8293 = ORIENTED_EDGE ( 'NONE', *, *, #11967, .T. ) ;
#8294 = CARTESIAN_POINT ( 'NONE',  ( -3.458734124999999437, 1.432654583217640498, 12.62500000136560629 ) ) ;
#8295 = CARTESIAN_POINT ( 'NONE',  ( 5.560781378645575757, 0.000000000000000000, -4.000000000000000000 ) ) ;
#8296 = CARTESIAN_POINT ( 'NONE',  ( -35.00000000000000000, 1.500000000000003109, -17.32050807568893092 ) ) ;
#8297 = DIRECTION ( 'NONE',  ( 0.000000000000000000, 0.000000000000000000, -1.000000000000000000 ) ) ;
#8298 = EDGE_CURVE ( 'NONE', #23552, #18582, #10130, .T. ) ;
#8299 = CARTESIAN_POINT ( 'NONE',  ( -71.45000000000000284, 12.50000000000000000, 13.96446609406725869 ) ) ;
#8300 = CARTESIAN_POINT ( 'NONE',  ( 48.67060293033276963, -11.25000000000000355, 5.000000000000079936 ) ) ;
#8301 = CARTESIAN_POINT ( 'NONE',  ( 59.87268183416157541, 7.219692298483935566, 12.12345345202367675 ) ) ;
#8302 = CARTESIAN_POINT ( 'NONE',  ( 9.000000000000000000, 0.000000000000000000, -1.102182119232617714E-15 ) ) ;
#8303 = CARTESIAN_POINT ( 'NONE',  ( 2.445694354108820967, -2.445694354108820079, 5.362500001365596347 ) ) ;
#8304 = LINE ( 'NONE', #6384, #18512 ) ;
#8305 = CARTESIAN_POINT ( 'NONE',  ( -1.656854249492379250, 4.000000000000000000, 12.93750000273119660 ) ) ;
#8306 = CARTESIAN_POINT ( 'NONE',  ( -19.99999999999999645, -9.000000000000003553, 5.000000000000079936 ) ) ;
#8307 = ORIENTED_EDGE ( 'NONE', *, *, #21132, .T. ) ;
#8308 = FACE_OUTER_BOUND ( 'NONE', #5019, .T. ) ;
#8309 = ORIENTED_EDGE ( 'NONE', *, *, #2334, .T. ) ;
#8310 = CARTESIAN_POINT ( 'NONE',  ( 53.68518183416157541, 10.06805114094562548, 11.99999999999999645 ) ) ;
#8311 = DIRECTION ( 'NONE',  ( 0.000000000000000000, 0.000000000000000000, 1.000000000000000000 ) ) ;
#8312 = EDGE_LOOP ( 'NONE', ( #8940, #9060, #13065, #20311 ) ) ;
#8313 = AXIS2_PLACEMENT_3D ( 'NONE', #16074, #23363, #2876 ) ;
#8314 = DIRECTION ( 'NONE',  ( -1.000000000000000000, 0.000000000000000000, 0.000000000000000000 ) ) ;
#8315 = VERTEX_POINT ( 'NONE', #21212 ) ;
#8316 = CARTESIAN_POINT ( 'NONE',  ( 72.50000000000000000, 9.999999999999998224, 14.99999999999999645 ) ) ;
#8317 = VERTEX_POINT ( 'NONE', #22790 ) ;
#8318 = CARTESIAN_POINT ( 'NONE',  ( 58.53356816583845301, 11.31069182806492712, 17.97181229448534623 ) ) ;
#8319 = B_SPLINE_CURVE_WITH_KNOTS ( 'NONE', 3,
 ( #23072, #7160, #21621, #12212, #3312, #17703 ),
 .UNSPECIFIED., .F., .F.,
 ( 4, 2, 4 ),
 ( 0.01049192114530184475, 0.01239128608052813933, 0.01429065101575443392 ),
 .UNSPECIFIED. ) ;
#8320 = AXIS2_PLACEMENT_3D ( 'NONE', #4925, #6843, #19881 ) ;
#8321 = CARTESIAN_POINT ( 'NONE',  ( -67.30000000218494449, 8.232233047033629347, 13.23223304703362402 ) ) ;
#8322 = CARTESIAN_POINT ( 'NONE',  ( -2.117863837641485618E-16, 3.458734125000000770, -2.262499998634403653 ) ) ;
#8323 = AXIS2_PLACEMENT_3D ( 'NONE', #23175, #3065, #3177 ) ;
#8324 = ADVANCED_FACE ( 'NONE', ( #15759 ), #14193, .T. ) ;
#8325 = ADVANCED_FACE ( 'NONE', ( #23029 ), #21451, .F. ) ;
#8326 = CARTESIAN_POINT ( 'NONE',  ( -4.211140560182196957, -2.431303136016552013, -3.745885042887436178 ) ) ;
#8327 =( BOUNDED_CURVE ( )  B_SPLINE_CURVE ( 2, ( #10815, #6835, #19521, #16184, #6963, #19633, #10581, #17852, #5272 ),
 .UNSPECIFIED., .F., .F. ) 
 B_SPLINE_CURVE_WITH_KNOTS ( ( 3, 2, 2, 2, 3 ),
 ( 0.5999999999999999778, 0.6125000000000000444, 0.6250000000000000000, 0.6374999999999999556, 0.6500000000000000222 ),
 .UNSPECIFIED. ) 
 CURVE ( )  GEOMETRIC_REPRESENTATION_ITEM ( )  RATIONAL_B_SPLINE_CURVE ( ( 1.000000000000000000, 0.9238795325112867385, 1.000000000000000000, 0.9238795325112867385, 1.000000000000000000, 0.9238795325112867385, 1.000000000000000000, 0.9238795325112867385, 1.000000000000000000 ) ) 
 REPRESENTATION_ITEM ( '' )  );
#8328 = CARTESIAN_POINT ( 'NONE',  ( 2.445694354108821411, 2.445694354108820523, 18.31250000136560274 ) ) ;
#8329 = ADVANCED_FACE ( 'NONE', ( #2901 ), #17423, .T. ) ;
#8330 = CARTESIAN_POINT ( 'NONE',  ( -2.828427124746188515, -2.828427124746190735, 15.25000000273119660 ) ) ;
#8331 = FACE_OUTER_BOUND ( 'NONE', #18190, .T. ) ;
#8332 = VECTOR ( 'NONE', #12577, 1000.000000000000000 ) ;
#8333 = CARTESIAN_POINT ( 'NONE',  ( 69.95000000109247651, 8.538419263543524096, 13.53841926354352054 ) ) ;
#8334 = CIRCLE ( 'NONE', #288, 12.00000000000000000 ) ;
#8335 = DIRECTION ( 'NONE',  ( 1.000000000000000000, -0.000000000000000000, -1.224646799147353454E-16 ) ) ;
#8336 = CARTESIAN_POINT ( 'NONE',  ( 52.62731816583844591, 12.16943976678978601, 17.07320092032949432 ) ) ;
#8337 = CARTESIAN_POINT ( 'NONE',  ( -1.432654583217640498, 3.458734125000000770, 2.800000001365598123 ) ) ;
#8338 = CARTESIAN_POINT ( 'NONE',  ( -3.458734124999999437, 0.000000000000000000, 10.68750000136560452 ) ) ;
#8339 = EDGE_CURVE ( 'NONE', #12043, #428, #4714, .T. ) ;
#8340 = CARTESIAN_POINT ( 'NONE',  ( -70.15000000109246514, 8.538419263543524096, 13.53841926354352054 ) ) ;
#8341 = LINE ( 'NONE', #19332, #1653 ) ;
#8342 = CARTESIAN_POINT ( 'NONE',  ( 65.80000000218494449, 9.999999999999998224, 12.49999999999999289 ) ) ;
#8343 = ORIENTED_EDGE ( 'NONE', *, *, #11733, .T. ) ;
#8344 = CARTESIAN_POINT ( 'NONE',  ( 72.50000000000000000, 9.999999999999998224, 12.49999999999999289 ) ) ;
#8345 = SURFACE_STYLE_FILL_AREA ( #13740 ) ;
#8346 = CARTESIAN_POINT ( 'NONE',  ( 7.347880794884118750E-16, -4.000000000000000000, 3.675000002731186211 ) ) ;
#8347 = ORIENTED_EDGE ( 'NONE', *, *, #18759, .T. ) ;
#8348 = VERTEX_POINT ( 'NONE', #1457 ) ;
#8349 = CIRCLE ( 'NONE', #16005, 6.000000000000021316 ) ;
#8350 = LINE ( 'NONE', #793, #3724 ) ;
#8351 = DIRECTION ( 'NONE',  ( 0.000000000000000000, 0.000000000000000000, -1.000000000000000000 ) ) ;
#8352 = ORIENTED_EDGE ( 'NONE', *, *, #17460, .F. ) ;
#8353 = CARTESIAN_POINT ( 'NONE',  ( 1.274258131564866448, 3.883108878240963513, -3.220599429844046568 ) ) ;
#8354 = AXIS2_PLACEMENT_3D ( 'NONE', #18492, #1608, #2075 ) ;
#8355 = PRODUCT_DEFINITION_CONTEXT ( 'detailed design', #2570, 'design' ) ;
#8356 = AXIS2_PLACEMENT_3D ( 'NONE', #15054, #20514, #7266 ) ;
#8357 = EDGE_CURVE ( 'NONE', #1384, #315, #14064, .T. ) ;
#8358 = CARTESIAN_POINT ( 'NONE',  ( 69.80000000109247082, 7.933012699999995476, 15.85617417291294196 ) ) ;
#8359 = CARTESIAN_POINT ( 'NONE',  ( 67.10000000109246798, 10.85617417291294551, 12.93301269999999370 ) ) ;
#8360 = ADVANCED_FACE ( 'NONE', ( #19662 ), #17882, .T. ) ;
#8361 = ORIENTED_EDGE ( 'NONE', *, *, #985, .F. ) ;
#8362 = CIRCLE ( 'NONE', #17540, 4.000000000000001776 ) ;
#8363 = CARTESIAN_POINT ( 'NONE',  ( 4.999999999999999112, 0.000000000000000000, 0.000000000000000000 ) ) ;
#8364 = CARTESIAN_POINT ( 'NONE',  ( 56.15625000000002132, 6.000000000000004441, 16.65685424949239390 ) ) ;
#8365 = CARTESIAN_POINT ( 'NONE',  ( 1.432654583217639832, 3.458734125000000326, 4.425000001365595459 ) ) ;
#8366 = EDGE_CURVE ( 'NONE', #14633, #21075, #824, .T. ) ;
#8367 = CARTESIAN_POINT ( 'NONE',  ( 66.65000000218496723, 11.03553390593276973, 12.50000000000002665 ) ) ;
#8368 = DIRECTION ( 'NONE',  ( 0.000000000000000000, 0.000000000000000000, 1.000000000000000000 ) ) ;
#8369 = CIRCLE ( 'NONE', #11443, 6.000000000000022204 ) ;
#8370 = EDGE_CURVE ( 'NONE', #20722, #19770, #8558, .T. ) ;
#8371 = CIRCLE ( 'NONE', #308, 4.000000000000001776 ) ;
#8372 = PLANE ( 'NONE',  #14787 ) ;
#8373 = ORIENTED_EDGE ( 'NONE', *, *, #5901, .F. ) ;
#8374 = DIRECTION ( 'NONE',  ( -1.000000000000000000, 0.000000000000000000, 0.000000000000000000 ) ) ;
#8375 = CARTESIAN_POINT ( 'NONE',  ( 0.000000000000000000, 0.000000000000000000, 0.000000000000000000 ) ) ;
#8376 = DIRECTION ( 'NONE',  ( -1.000000000000000000, 0.000000000000000000, 1.239088197126290817E-16 ) ) ;
#8377 = ORIENTED_EDGE ( 'NONE', *, *, #5733, .F. ) ;
#8378 = DIRECTION ( 'NONE',  ( 0.000000000000000000, 0.000000000000000000, -1.000000000000000000 ) ) ;
#8379 = DIRECTION ( 'NONE',  ( 0.000000000000000000, 0.000000000000000000, 1.000000000000000000 ) ) ;
#8380 = DIRECTION ( 'NONE',  ( 0.3420201433256622736, -0.9396926207859106484, -1.232595164407828100E-31 ) ) ;
#8381 = ORIENTED_EDGE ( 'NONE', *, *, #5901, .T. ) ;
#8382 = CARTESIAN_POINT ( 'NONE',  ( 33.85151041966726382, -11.25000000000000355, 10.00000000000008882 ) ) ;
#8383 = ORIENTED_EDGE ( 'NONE', *, *, #22970, .T. ) ;
#8384 = AXIS2_PLACEMENT_3D ( 'NONE', #15235, #18805, #2271 ) ;
#8385 = CARTESIAN_POINT ( 'NONE',  ( 71.95000000109247651, 11.46158073645647235, 16.46158073645647235 ) ) ;
#8386 = DIRECTION ( 'NONE',  ( -1.000000000000000000, 0.000000000000000000, 0.000000000000000000 ) ) ;
#8387 = CARTESIAN_POINT ( 'NONE',  ( -5.432802636760778903, 4.368923434677189910, -0.2573354458087841468 ) ) ;
#8388 = AXIS2_PLACEMENT_3D ( 'NONE', #6580, #19722, #8505 ) ;
#8389 = LINE ( 'NONE', #11879, #15624 ) ;
#8390 = CARTESIAN_POINT ( 'NONE',  ( 68.15000000109246514, 11.46158073645647235, 16.46158073645647235 ) ) ;
#8391 = ORIENTED_EDGE ( 'NONE', *, *, #5375, .T. ) ;
#8392 = CARTESIAN_POINT ( 'NONE',  ( 72.50000000000000000, 9.999999999999998224, 17.49999999999999645 ) ) ;
#8393 = EDGE_CURVE ( 'NONE', #22113, #19299, #23141, .T. ) ;
#8394 = FACE_OUTER_BOUND ( 'NONE', #10219, .T. ) ;
#8396 = ADVANCED_FACE ( 'NONE', ( #12285 ), #10952, .F. ) ;
#8395 = AXIS2_PLACEMENT_3D ( 'NONE', #21432, #5162, #1677 ) ;
#8397 = CARTESIAN_POINT ( 'NONE',  ( 71.10000000109246798, 10.85617417291294551, 12.93301269999999370 ) ) ;
#8398 = CARTESIAN_POINT ( 'NONE',  ( -1.432654583217639166, 3.458734125000000770, 17.50000000136560274 ) ) ;
#8399 = CARTESIAN_POINT ( 'NONE',  ( 72.50000000000000000, 9.999999999999998224, 14.99999999999999645 ) ) ;
#8400 = EDGE_CURVE ( 'NONE', #7146, #13567, #19379, .T. ) ;
#8401 = AXIS2_PLACEMENT_3D ( 'NONE', #14137, #21403, #22858 ) ;
#8402 = DIRECTION ( 'NONE',  ( -0.000000000000000000, 0.000000000000000000, -1.000000000000000000 ) ) ;
#8403 = SHAPE_REPRESENTATION ( 'BR-005', ( #5718, #6066, #19435, #9156, #20488, #14150, #22146, #3411, #8029, #8410, #19104, #4953, #8803, #13011, #21754, #6099, #1875, #11873, #7633, #1486, #2653, #17944 ), #347 ) ;
#8404 = VERTEX_POINT ( 'NONE', #5304 ) ;
#8405 = CARTESIAN_POINT ( 'NONE',  ( -2.828427124746190291, 2.828427124746190291, -0.8249999999999976241 ) ) ;
#8406 = B_SPLINE_CURVE_WITH_KNOTS ( 'NONE', 3,
 ( #314, #1755, #9439, #19839, #3445, #1869 ),
 .UNSPECIFIED., .F., .F.,
 ( 4, 2, 4 ),
 ( 0.006695446894088488872, 0.008593684019695166376, 0.01049192114530184301 ),
 .UNSPECIFIED. ) ;
#8407 = CARTESIAN_POINT ( 'NONE',  ( 65.75000000109245946, 9.999999999999998224, 17.49999999999999645 ) ) ;
#8408 = DIRECTION ( 'NONE',  ( -1.000000000000000000, -0.000000000000000000, -0.000000000000000000 ) ) ;
#8409 = CARTESIAN_POINT ( 'NONE',  ( 1.506022603841227436, 1.012170579495290078E-15, 8.265000000000021885 ) ) ;
#8410 = AXIS2_PLACEMENT_3D ( 'NONE', #9155, #5058, #14423 ) ;
#8411 = ORIENTED_EDGE ( 'NONE', *, *, #4401, .F. ) ;
#8413 = LINE ( 'NONE', #19626, #23138 ) ;
#8412 = AXIS2_PLACEMENT_3D ( 'NONE', #10091, #8169, #22870 ) ;
#8414 = EDGE_LOOP ( 'NONE', ( #21266, #6448, #19522, #8753 ) ) ;
#8415 = CARTESIAN_POINT ( 'NONE',  ( -66.70000000109246230, 9.143825827087049163, 17.06698729999999742 ) ) ;
#8416 = VECTOR ( 'NONE', #1320, 1000.000000000000000 ) ;
#8417 = ORIENTED_EDGE ( 'NONE', *, *, #7967, .T. ) ;
#8418 = CARTESIAN_POINT ( 'NONE',  ( 1.656854249492380138, 4.000000000000000000, -1.887499997268811791 ) ) ;
#8419 = ORIENTED_EDGE ( 'NONE', *, *, #4860, .T. ) ;
#8420 = ORIENTED_EDGE ( 'NONE', *, *, #15114, .T. ) ;
#8421 = CARTESIAN_POINT ( 'NONE',  ( -3.458734124999998993, -1.432654583217642497, 13.75000000136560452 ) ) ;
#8422 = CIRCLE ( 'NONE', #19094, 4.714285714285714413 ) ;
#8423 = DIRECTION ( 'NONE',  ( 0.000000000000000000, 0.000000000000000000, -1.000000000000000000 ) ) ;
#8424 = AXIS2_PLACEMENT_3D ( 'NONE', #4513, #9930, #13878 ) ;
#8425 = CARTESIAN_POINT ( 'NONE',  ( -3.847601380332740018, -11.25000000000000355, 10.00000000000008882 ) ) ;
#8426 = CARTESIAN_POINT ( 'NONE',  ( 66.25000000109247367, 12.06698730000000097, 14.99999999999999645 ) ) ;
#8427 = CARTESIAN_POINT ( 'NONE',  ( -69.84999999999999432, 12.50000000000000000, 13.96446609406725869 ) ) ;
#8428 = AXIS2_PLACEMENT_3D ( 'NONE', #5196, #14568, #19563 ) ;
#8429 = EDGE_CURVE ( 'NONE', #13424, #17245, #16101, .T. ) ;
#8430 = DIRECTION ( 'NONE',  ( 0.000000000000000000, -0.3090169943749551673, 0.9510565162951511997 ) ) ;
#8431 = CARTESIAN_POINT ( 'NONE',  ( 57.71643183416158251, 13.97181229448536399, 16.72490539043799629 ) ) ;
#8432 = DIRECTION ( 'NONE',  ( -0.000000000000000000, 1.000000000000000000, -0.000000000000000000 ) ) ;
#8433 = CARTESIAN_POINT ( 'NONE',  ( 3.458734125000000770, 4.235727675282972223E-16, 1.487500001365596125 ) ) ;
#8434 = CARTESIAN_POINT ( 'NONE',  ( -67.45000000218493597, 11.03553390593273420, 12.49999999999998934 ) ) ;
#8435 = DIRECTION ( 'NONE',  ( 0.000000000000000000, 0.000000000000000000, 1.000000000000000000 ) ) ;
#8436 = CARTESIAN_POINT ( 'NONE',  ( 2.828427124746191179, 2.828427124746190291, 12.75000000273119660 ) ) ;
#8437 = CARTESIAN_POINT ( 'NONE',  ( -20.00000000000000711, 9.999999999999964473, -19.99999999999999645 ) ) ;
#8438 = AXIS2_PLACEMENT_3D ( 'NONE', #507, #20496, #7829 ) ;
#8439 = CIRCLE ( 'NONE', #9585, 12.00000000000000000 ) ;
#8440 = ORIENTED_EDGE ( 'NONE', *, *, #3399, .F. ) ;
#8441 = CARTESIAN_POINT ( 'NONE',  ( -70.90000000109247935, 10.85617417291294551, 12.93301269999999192 ) ) ;
#8442 = ORIENTED_EDGE ( 'NONE', *, *, #13905, .T. ) ;
#8443 = CARTESIAN_POINT ( 'NONE',  ( 60.62268183416157541, 12.78030770151606177, 17.87654654797631792 ) ) ;
#8444 = SURFACE_STYLE_FILL_AREA ( #17177 ) ;
#8445 = CARTESIAN_POINT ( 'NONE',  ( 1.432654583217639832, 3.458734125000000326, 1.425000001365597013 ) ) ;
#8446 = VERTEX_POINT ( 'NONE', #2046 ) ;
#8447 = CIRCLE ( 'NONE', #3447, 8.239200000000002078 ) ;
#8448 = DIRECTION ( 'NONE',  ( 1.000000000000000000, 0.000000000000000000, 0.000000000000000000 ) ) ;
#8449 = EDGE_CURVE ( 'NONE', #6753, #4288, #3705, .T. ) ;
#8450 = AXIS2_PLACEMENT_3D ( 'NONE', #7457, #5520, #126 ) ;
#8451 = ORIENTED_EDGE ( 'NONE', *, *, #13190, .T. ) ;
#8452 = DIRECTION ( 'NONE',  ( 0.000000000000000000, 0.000000000000000000, 1.000000000000000000 ) ) ;
#8453 = ORIENTED_EDGE ( 'NONE', *, *, #2171, .F. ) ;
#8454 = CARTESIAN_POINT ( 'NONE',  ( 50.47106816583844591, 5.971812294485345340, 13.41119689145326710 ) ) ;
#8455 = CARTESIAN_POINT ( 'NONE',  ( -67.90000000218495302, 8.232233047033627571, 16.76776695296636532 ) ) ;
#8456 = CARTESIAN_POINT ( 'NONE',  ( 31.53809564071656624, -8.974600000000002353, 5.000000000000079936 ) ) ;
#8457 = CARTESIAN_POINT ( 'NONE',  ( 1.506022603841296714, 0.000000000000000000, -6.735000000000022524 ) ) ;
#8458 = CARTESIAN_POINT ( 'NONE',  ( -3.458734124999999437, 0.000000000000000000, 17.68750000136560274 ) ) ;
#8459 = CARTESIAN_POINT ( 'NONE',  ( 1.656854249492381470, 4.000000000000000000, 13.81250000273119483 ) ) ;
#8460 = CARTESIAN_POINT ( 'NONE',  ( 58.68750000000000000, 9.999999999999989342, 11.99999999999999467 ) ) ;
#8461 = AXIS2_PLACEMENT_3D ( 'NONE', #6060, #17083, #8228 ) ;
#8462 = CARTESIAN_POINT ( 'NONE',  ( 68.45000000109247651, 9.999999999999998224, 12.93301269999999192 ) ) ;
#8463 = CARTESIAN_POINT ( 'NONE',  ( 70.60000000218494165, 9.999999999999998224, 12.49999999999999289 ) ) ;
#8464 = CIRCLE ( 'NONE', #8842, 2.041999999999999815 ) ;
#8465 = CARTESIAN_POINT ( 'NONE',  ( 50.00231816583843170, 12.07320092032949610, 12.83056023321021044 ) ) ;
#8466 = CARTESIAN_POINT ( 'NONE',  ( 6.353591512924457348E-16, -3.458734125000000770, 3.237500001365597679 ) ) ;
#8467 = CARTESIAN_POINT ( 'NONE',  ( -1.432654583217639166, 3.458734125000000770, 12.50000000136560452 ) ) ;
#8468 = CARTESIAN_POINT ( 'NONE',  ( -6.500000000000000000, -3.752776749732572359, -3.700000000000000178 ) ) ;
#8469 = CARTESIAN_POINT ( 'NONE',  ( -68.90000000109246514, 12.06698729999999919, 15.85617417291294196 ) ) ;
#8470 = VERTEX_POINT ( 'NONE', #23386 ) ;
#8471 = CARTESIAN_POINT ( 'NONE',  ( -60.00000000000000711, 15.00000000000000000, 10.00000000000004974 ) ) ;
#8472 = LINE ( 'NONE', #17445, #930 ) ;
#8473 = VERTEX_POINT ( 'NONE', #11192 ) ;
#8474 = CARTESIAN_POINT ( 'NONE',  ( 59.53125000000000000, 11.24264068711929276, 18.00000000000000355 ) ) ;
#8475 = CARTESIAN_POINT ( 'NONE',  ( 1.656854249492383024, -3.999999999999999112, 1.737500002731187543 ) ) ;
#8476 = EDGE_LOOP ( 'NONE', ( #3116, #6720, #10215, #2867 ) ) ;
#8477 = EDGE_LOOP ( 'NONE', ( #1985, #408, #11663 ) ) ;
#8478 = EDGE_CURVE ( 'NONE', #18582, #7791, #16442, .T. ) ;
#8479 = CARTESIAN_POINT ( 'NONE',  ( 45.00000000000000000, 2.399706452296353820, 60.00000000000021316 ) ) ;
#8480 = CARTESIAN_POINT ( 'NONE',  ( -4.736472119667250347, -11.25000000000000355, 5.000000000000079936 ) ) ;
#8481 = ORIENTED_EDGE ( 'NONE', *, *, #13199, .F. ) ;
#8482 = CARTESIAN_POINT ( 'NONE',  ( 118.3095189484530181, -10.00000000000001954, 17.50000000000003553 ) ) ;
#8483 = AXIS2_PLACEMENT_3D ( 'NONE', #19618, #14384, #15823 ) ;
#8484 = EDGE_CURVE ( 'NONE', #5362, #1913, #19784, .T. ) ;
#8485 = CARTESIAN_POINT ( 'NONE',  ( 69.50000000109248788, 12.06698730000000275, 15.85617417291294196 ) ) ;
#8486 = CARTESIAN_POINT ( 'NONE',  ( 67.35000000109246798, 11.46158073645647235, 16.46158073645647235 ) ) ;
#8487 = CARTESIAN_POINT ( 'NONE',  ( 2.828427124746192067, -2.828427124746189847, 17.50000000273119483 ) ) ;
#8488 = FACE_OUTER_BOUND ( 'NONE', #9246, .T. ) ;
#8489 = CARTESIAN_POINT ( 'NONE',  ( 58.21875000000000711, 14.00000000000000888, 16.65685424949235482 ) ) ;
#8490 = CARTESIAN_POINT ( 'NONE',  ( -3.458734125000000326, 1.432654583217640276, 3.675000001365593238 ) ) ;
#8491 = CARTESIAN_POINT ( 'NONE',  ( 1.432654583217641164, 3.458734125000000326, 15.12500000136560807 ) ) ;
#8492 = DIRECTION ( 'NONE',  ( 1.000000000000000000, 7.703719777548943412E-32, 0.000000000000000000 ) ) ;
#8493 = CARTESIAN_POINT ( 'NONE',  ( -1.600000000000004086, 0.000000000000000000, 0.000000000000000000 ) ) ;
#8494 = ORIENTED_EDGE ( 'NONE', *, *, #17769, .F. ) ;
#8495 = CYLINDRICAL_SURFACE ( 'NONE', #7, 2.500000000000002220 ) ;
#8496 = DIRECTION ( 'NONE',  ( -1.000000000000000000, 0.000000000000000000, -0.000000000000000000 ) ) ;
#8497 = CARTESIAN_POINT ( 'NONE',  ( 4.999999999999999112, 2.223716399045570835, 8.461683424509324425 ) ) ;
#8498 = ORIENTED_EDGE ( 'NONE', *, *, #8210, .T. ) ;
#8499 = ADVANCED_FACE ( 'NONE', ( #16330 ), #1694, .F. ) ;
#8500 = CARTESIAN_POINT ( 'NONE',  ( 0.000000000000000000, -8.152713396088785203, 3.174628368996045946 ) ) ;
#8501 = CARTESIAN_POINT ( 'NONE',  ( 71.70000000109247651, 10.85617417291294551, 12.93301269999999370 ) ) ;
#8502 = EDGE_CURVE ( 'NONE', #12637, #20551, #21820, .T. ) ;
#8503 = DIRECTION ( 'NONE',  ( -1.000000000000000000, 0.000000000000000000, -0.000000000000000000 ) ) ;
#8504 = ORIENTED_EDGE ( 'NONE', *, *, #18112, .T. ) ;
#8505 = DIRECTION ( 'NONE',  ( 0.000000000000000000, 0.000000000000000000, -1.000000000000000000 ) ) ;
#8506 = ORIENTED_EDGE ( 'NONE', *, *, #17253, .F. ) ;
#8507 = FACE_OUTER_BOUND ( 'NONE', #23110, .T. ) ;
#8508 = ADVANCED_FACE ( 'NONE', ( #21692 ), #20137, .T. ) ;
#8509 = CARTESIAN_POINT ( 'NONE',  ( 70.75000000218496155, 12.50000000000000000, 13.96446609406725869 ) ) ;
#8510 = EDGE_CURVE ( 'NONE', #13902, #22997, #2167, .T. ) ;
#8511 = DIRECTION ( 'NONE',  ( 0.000000000000000000, 0.000000000000000000, -1.000000000000000000 ) ) ;
#8512 = LINE ( 'NONE', #6697, #14850 ) ;
#8513 = CARTESIAN_POINT ( 'NONE',  ( 68.75000000109245946, 11.46158073645647235, 13.53841926354352232 ) ) ;
#8514 = ORIENTED_EDGE ( 'NONE', *, *, #4824, .T. ) ;
#8515 = CARTESIAN_POINT ( 'NONE',  ( -54.99999999999992895, 15.00000000000000000, 1.387778780781445676E-14 ) ) ;
#8516 = DIRECTION ( 'NONE',  ( 0.9396926207859107594, -0.3420201433256623291, 3.697785493223492838E-32 ) ) ;
#8517 = CARTESIAN_POINT ( 'NONE',  ( 66.15000000109247935, 8.538419263543524096, 13.53841926354352054 ) ) ;
#8518 = CARTESIAN_POINT ( 'NONE',  ( 1.432654583217643163, -3.458734124999999437, 10.75000000136560452 ) ) ;
#8519 = DIRECTION ( 'NONE',  ( 1.000000000000000000, 7.703719777548943412E-32, 0.000000000000000000 ) ) ;
#8520 = ORIENTED_EDGE ( 'NONE', *, *, #16413, .T. ) ;
#8521 = CARTESIAN_POINT ( 'NONE',  ( -1.656854249492381248, -3.999999999999999112, -2.512499999999998401 ) ) ;
#8522 = LINE ( 'NONE', #6710, #15920 ) ;
#8523 = CARTESIAN_POINT ( 'NONE',  ( 2.828427124746190735, -2.828427124746189847, 0.8000000027311872097 ) ) ;
#8524 = CONICAL_SURFACE ( 'NONE', #11595, 6.735000000000022524, 0.4459949661726533843 ) ;
#8525 = CARTESIAN_POINT ( 'NONE',  ( 1.734723475976807094E-15, 4.618802153517012954, -0.4999999999999995559 ) ) ;
#8526 = EDGE_LOOP ( 'NONE', ( #13437, #21287, #18144, #23383 ) ) ;
#8527 = DIRECTION ( 'NONE',  ( 0.000000000000000000, 0.000000000000000000, -1.000000000000000000 ) ) ;
#8528 = ORIENTED_EDGE ( 'NONE', *, *, #13220, .F. ) ;
#8529 = CARTESIAN_POINT ( 'NONE',  ( -6.500000000000000000, 0.000000000000000000, 1.734723475976807094E-15 ) ) ;
#8530 = EDGE_CURVE ( 'NONE', #17536, #9561, #12646, .T. ) ;
#8531 = VERTEX_POINT ( 'NONE', #18354 ) ;
#8532 = CARTESIAN_POINT ( 'NONE',  ( -4.101948962585906244, 2.368261337751074169, -3.681124513963621503 ) ) ;
#8533 = ORIENTED_EDGE ( 'NONE', *, *, #11760, .T. ) ;
#8534 = ORIENTED_EDGE ( 'NONE', *, *, #22795, .T. ) ;
#8535 = CARTESIAN_POINT ( 'NONE',  ( 2.445694354108821411, 2.445694354108820523, 14.31250000136560452 ) ) ;
#8536 = CARTESIAN_POINT ( 'NONE',  ( -35.00000000000000000, 7.500000000000001776, -19.99999999999998934 ) ) ;
#8537 = ADVANCED_FACE ( 'NONE', ( #10841 ), #3273, .T. ) ;
#8538 = CARTESIAN_POINT ( 'NONE',  ( 0.000000000000000000, 0.000000000000000000, 0.000000000000000000 ) ) ;
#8539 = CARTESIAN_POINT ( 'NONE',  ( 67.05000000109247082, 12.06698730000000097, 14.99999999999999645 ) ) ;
#8540 = CARTESIAN_POINT ( 'NONE',  ( -71.09999999999999432, 7.499999999999996447, 14.99999999999999645 ) ) ;
#8541 = DIRECTION ( 'NONE',  ( 1.000000000000000000, 0.000000000000000000, 0.000000000000000000 ) ) ;
#8542 = CARTESIAN_POINT ( 'NONE',  ( 60.00000000000002842, 11.59862743136960717, 18.35022190915677243 ) ) ;
#8543 = CARTESIAN_POINT ( 'NONE',  ( -3.458734125000000326, -1.432654583217642497, 1.050000001365596791 ) ) ;
#8544 = CARTESIAN_POINT ( 'NONE',  ( 67.10000000218495586, 8.232233047033627571, 16.76776695296636532 ) ) ;
#8545 = DIRECTION ( 'NONE',  ( -1.000000000000000000, -0.000000000000000000, -0.000000000000000000 ) ) ;
#8546 = CARTESIAN_POINT ( 'NONE',  ( 2.445694354108821411, 2.445694354108820523, 18.06250000136560274 ) ) ;
#8547 = DIRECTION ( 'NONE',  ( -1.000000000000000000, -8.881784197001252323E-16, 0.000000000000000000 ) ) ;
#8548 = EDGE_LOOP ( 'NONE', ( #15549, #16893 ) ) ;
#8549 = CARTESIAN_POINT ( 'NONE',  ( -2.828427124746188515, -2.828427124746190735, 14.25000000273119660 ) ) ;
#8550 = EDGE_LOOP ( 'NONE', ( #11533, #1709, #7959, #18276 ) ) ;
#8551 = CARTESIAN_POINT ( 'NONE',  ( 54.90393183416157541, 13.02818770551463778, 13.82541045382633982 ) ) ;
#8552 = CARTESIAN_POINT ( 'NONE',  ( -1.432654583217640276, 3.458734125000000326, -1.449999998634403875 ) ) ;
#8553 = VERTEX_POINT ( 'NONE', #23418 ) ;
#8554 = CARTESIAN_POINT ( 'NONE',  ( 0.000000000000000000, 0.000000000000000000, 19.04999999999996874 ) ) ;
#8555 = VECTOR ( 'NONE', #13852, 1000.000000000000000 ) ;
#8556 = CIRCLE ( 'NONE', #17340, 8.749000000000002331 ) ;
#8557 = ORIENTED_EDGE ( 'NONE', *, *, #2051, .F. ) ;
#8558 = LINE ( 'NONE', #13843, #23209 ) ;
#8559 = ORIENTED_EDGE ( 'NONE', *, *, #7202, .F. ) ;
#8560 = EDGE_CURVE ( 'NONE', #19450, #15217, #3174, .T. ) ;
#8561 = CARTESIAN_POINT ( 'NONE',  ( 56.28356816583844591, 8.689308171935074654, 12.02818770551464489 ) ) ;
#8562 = CARTESIAN_POINT ( 'NONE',  ( -66.65000000218493881, 11.03553390593273598, 12.49999999999999289 ) ) ;
#8563 = PLANE ( 'NONE',  #19771 ) ;
#8564 = CARTESIAN_POINT ( 'NONE',  ( -4.714285714285714413, 5.773334910266094008E-16, 9.480888224575631185 ) ) ;
#8565 = CARTESIAN_POINT ( 'NONE',  ( 1.872352939448454495E-15, -3.458734125000000770, 13.93750000136560629 ) ) ;
#8566 = CARTESIAN_POINT ( 'NONE',  ( 4.000000000000000888, 1.656854249492381248, 14.68750000273119660 ) ) ;
#8567 = CARTESIAN_POINT ( 'NONE',  ( 59.06250000000000711, 6.999999999999997335, 15.00000000000000533 ) ) ;
#8568 = CARTESIAN_POINT ( 'NONE',  ( 4.999999999999999112, 9.241976615262160522, 2.300561732649595736 ) ) ;
#8569 = VECTOR ( 'NONE', #12793, 1000.000000000000000 ) ;
#8570 = CARTESIAN_POINT ( 'NONE',  ( 58.21875000000000711, 13.00000000000000711, 16.24264068711927322 ) ) ;
#8571 = CARTESIAN_POINT ( 'NONE',  ( -2.445694354108820523, 2.445694354108820523, 1.862500001365596347 ) ) ;
#8572 = CARTESIAN_POINT ( 'NONE',  ( 3.458734125000001658, 4.235727675282972223E-16, 12.18750000136560629 ) ) ;
#8573 = CARTESIAN_POINT ( 'NONE',  ( 67.70000000000000284, 9.999999999999998224, 17.49999999999999645 ) ) ;
#8574 = CARTESIAN_POINT ( 'NONE',  ( -68.55000000109247082, 8.538419263543524096, 13.53841926354352054 ) ) ;
#8575 = ORIENTED_EDGE ( 'NONE', *, *, #13667, .T. ) ;
#8576 = LINE ( 'NONE', #14325, #2929 ) ;
#8577 = CARTESIAN_POINT ( 'NONE',  ( 8.718769219667262149, -11.25000000000000355, 10.00000000000008882 ) ) ;
#8578 = VERTEX_POINT ( 'NONE', #6346 ) ;
#8579 = CARTESIAN_POINT ( 'NONE',  ( 58.50000000000000000, 12.12132034355963484, 12.87867965644034740 ) ) ;
#8580 =( LENGTH_UNIT ( ) NAMED_UNIT ( * ) SI_UNIT ( .MILLI., .METRE. ) );
#8581 = CARTESIAN_POINT ( 'NONE',  ( 2.828427124746190735, -2.828427124746189847, -1.199999997268811125 ) ) ;
#8582 = ORIENTED_EDGE ( 'NONE', *, *, #21922, .T. ) ;
#8583 = ORIENTED_EDGE ( 'NONE', *, *, #18724, .F. ) ;
#8584 = CARTESIAN_POINT ( 'NONE',  ( 0.5303295852573084446, -7.199367570657613236, -0.4037800551813831573 ) ) ;
#8585 = FACE_OUTER_BOUND ( 'NONE', #15166, .T. ) ;
#8586 = VERTEX_POINT ( 'NONE', #21602 ) ;
#8587 = DIRECTION ( 'NONE',  ( 0.000000000000000000, 0.000000000000000000, -1.000000000000000000 ) ) ;
#8588 = UNCERTAINTY_MEASURE_WITH_UNIT (LENGTH_MEASURE( 1.000000000000000082E-05 ), #14527, 'distance_accuracy_value', 'NONE');
#8589 = CARTESIAN_POINT ( 'NONE',  ( -69.45000000218495018, 8.964466094067256918, 17.49999999999999289 ) ) ;
#8590 = CARTESIAN_POINT ( 'NONE',  ( 0.000000000000000000, -6.807171995660539210, -6.478011392632959442 ) ) ;
#8591 = CARTESIAN_POINT ( 'NONE',  ( 66.25000000109245946, 9.999999999999998224, 12.93301269999999192 ) ) ;
#8592 = DIRECTION ( 'NONE',  ( -1.000000000000000000, 0.000000000000000000, 0.000000000000000000 ) ) ;
#8593 = EDGE_CURVE ( 'NONE', #14452, #4468, #8706, .T. ) ;
#8595 = FACE_OUTER_BOUND ( 'NONE', #18849, .T. ) ;
#8594 = AXIS2_PLACEMENT_3D ( 'NONE', #6302, #22581, #6660 ) ;
#8596 = CARTESIAN_POINT ( 'NONE',  ( 57.59606816583843880, 11.58880310854672935, 10.97181229448534445 ) ) ;
#8597 = CARTESIAN_POINT ( 'NONE',  ( -2.117863837641485618E-16, 3.458734125000000326, 5.487500001365596347 ) ) ;
#8598 = CARTESIAN_POINT ( 'NONE',  ( -3.458734124999998105, 1.432654583217640276, 13.37500000136560274 ) ) ;
#8599 = DIRECTION ( 'NONE',  ( -1.000000000000000000, -0.000000000000000000, -0.000000000000000000 ) ) ;
#8600 = LINE ( 'NONE', #21499, #13245 ) ;
#8601 = ORIENTED_EDGE ( 'NONE', *, *, #10989, .T. ) ;
#8602 = CARTESIAN_POINT ( 'NONE',  ( -1.800000000000000711, 0.000000000000000000, -8.800000000000022027 ) ) ;
#8603 = CARTESIAN_POINT ( 'NONE',  ( -0.7060087303327398089, -11.25000000000000355, 5.000000000000079936 ) ) ;
#8604 = CARTESIAN_POINT ( 'NONE',  ( -20.00000000000001066, 16.40063509461079150, -43.12916512459904084 ) ) ;
#8605 = EDGE_CURVE ( 'NONE', #18572, #10729, #12554, .T. ) ;
#8606 = ORIENTED_EDGE ( 'NONE', *, *, #23226, .F. ) ;
#8607 = CARTESIAN_POINT ( 'NONE',  ( 9.920644283265380691E-16, 4.000000000000000000, 13.87500000273119483 ) ) ;
#8608 = FACE_OUTER_BOUND ( 'NONE', #2543, .T. ) ;
#8609 = DIRECTION ( 'NONE',  ( -1.000000000000000000, 0.000000000000000000, 0.000000000000000000 ) ) ;
#8610 = EDGE_LOOP ( 'NONE', ( #18545, #13511, #18789, #16045 ) ) ;
#8611 = CARTESIAN_POINT ( 'NONE',  ( -69.59999999999999432, 8.232233047033629347, 13.23223304703362402 ) ) ;
#8612 = ORIENTED_EDGE ( 'NONE', *, *, #252, .F. ) ;
#8613 = AXIS2_PLACEMENT_3D ( 'NONE', #10455, #6959, #17965 ) ;
#8614 = CARTESIAN_POINT ( 'NONE',  ( 58.62731816583843170, 12.87654654797634102, 17.78030770151602979 ) ) ;
#8615 = AXIS2_PLACEMENT_3D ( 'NONE', #16345, #7255, #10507 ) ;
#8616 = AXIS2_PLACEMENT_3D ( 'NONE', #5609, #18419, #1998 ) ;
#8617 = CARTESIAN_POINT ( 'NONE',  ( 68.75000000218496155, 7.499999999999995559, 16.03553390593273420 ) ) ;
#8618 = CARTESIAN_POINT ( 'NONE',  ( -2.828427124746189403, 2.828427124746190291, 11.87500000000001066 ) ) ;
#8619 = CARTESIAN_POINT ( 'NONE',  ( 67.85000000109246798, 9.999999999999998224, 12.93301269999999192 ) ) ;
#8620 = ORIENTED_EDGE ( 'NONE', *, *, #16954, .T. ) ;
#8621 = ADVANCED_FACE ( 'NONE', ( #5093 ), #22437, .F. ) ;
#8622 = CARTESIAN_POINT ( 'NONE',  ( -68.85000000218495586, 7.499999999999996447, 13.96446609406725514 ) ) ;
#8623 = EDGE_CURVE ( 'NONE', #22275, #5838, #11755, .T. ) ;
#8624 = LINE ( 'NONE', #6590, #1099 ) ;
#8625 = CARTESIAN_POINT ( 'NONE',  ( 66.60000000109246798, 10.85617417291294551, 17.06698729999999742 ) ) ;
#8626 = CARTESIAN_POINT ( 'NONE',  ( 3.458734125000002102, -1.432654583217639610, 10.87500000136560452 ) ) ;
#8627 = DIRECTION ( 'NONE',  ( 1.000000000000000000, 0.000000000000000000, 0.000000000000000000 ) ) ;
#8628 = CONICAL_SURFACE ( 'NONE', #9777, 2.041999999999999815, 1.047197551196591858 ) ;
#8629 = CARTESIAN_POINT ( 'NONE',  ( -6.500000000000000000, -3.752776749732573247, -3.119443416399232394 ) ) ;
#8630 = EDGE_LOOP ( 'NONE', ( #20970, #22871, #1754, #20796 ) ) ;
#8631 = CARTESIAN_POINT ( 'NONE',  ( -35.00000000000000000, -8.499999999999966249, 1.285879139104720791E-14 ) ) ;
#8632 = CARTESIAN_POINT ( 'NONE',  ( 55.31250000000000711, 13.00000000000000000, 14.99999999999998757 ) ) ;
#8633 = AXIS2_PLACEMENT_3D ( 'NONE', #11711, #296, #20657 ) ;
#8634 = CARTESIAN_POINT ( 'NONE',  ( 0.000000000000000000, -1.975651141462162474, -10.82112760146738673 ) ) ;
#8635 = EDGE_CURVE ( 'NONE', #21124, #5860, #191, .T. ) ;
#8636 = ORIENTED_EDGE ( 'NONE', *, *, #18431, .T. ) ;
#8637 = CARTESIAN_POINT ( 'NONE',  ( -3.458734124999998993, 0.000000000000000000, 19.43750000136560629 ) ) ;
#8638 = CARTESIAN_POINT ( 'NONE',  ( -1.432654583217640942, -3.458734124999999882, -0.07499999863440427739 ) ) ;
#8639 = CARTESIAN_POINT ( 'NONE',  ( 2.855764796983346177, -2.970025579236428737, -0.09382832055446485575 ) ) ;
#8640 = VERTEX_POINT ( 'NONE', #6781 ) ;
#8641 = FACE_OUTER_BOUND ( 'NONE', #22582, .T. ) ;
#8642 = ORIENTED_EDGE ( 'NONE', *, *, #16405, .T. ) ;
#8643 = DIRECTION ( 'NONE',  ( -0.000000000000000000, -0.000000000000000000, 1.000000000000000000 ) ) ;
#8644 = ORIENTED_EDGE ( 'NONE', *, *, #16909, .T. ) ;
#8645 = CARTESIAN_POINT ( 'NONE',  ( 1.432654583217643163, -3.458734124999999882, 11.00000000136560452 ) ) ;
#8646 = DIRECTION ( 'NONE',  ( 1.000000000000000000, 7.703719777548943412E-32, 0.000000000000000000 ) ) ;
#8647 = AXIS2_PLACEMENT_3D ( 'NONE', #23025, #15754, #8311 ) ;
#8648 = VECTOR ( 'NONE', #4201, 1000.000000000000000 ) ;
#8649 = CARTESIAN_POINT ( 'NONE',  ( -66.90000000218495302, 11.76776695296636888, 16.76776695296636532 ) ) ;
#8650 = ADVANCED_FACE ( 'NONE', ( #21365 ), #4987, .T. ) ;
#8651 = CONICAL_SURFACE ( 'NONE', #21950, 6.735000000000022524, 0.4459949661726533843 ) ;
#8652 = CARTESIAN_POINT ( 'NONE',  ( 66.35000000109248219, 11.46158073645647235, 16.46158073645647235 ) ) ;
#8653 = CARTESIAN_POINT ( 'NONE',  ( 5.577176569667260608, -11.25000000000000355, 5.000000000000079936 ) ) ;
#8654 = CARTESIAN_POINT ( 'NONE',  ( -71.54999999999999716, 12.50000000000000000, 16.03553390593273420 ) ) ;
#8655 = ADVANCED_FACE ( 'NONE', ( #7619 ), #22194, .T. ) ;
#8656 = CARTESIAN_POINT ( 'NONE',  ( 50.00000000000000000, 14.69846310392956745, 35.82846581308617573 ) ) ;
#8657 = CARTESIAN_POINT ( 'NONE',  ( 59.99999999999998579, 10.91440514551900698, 18.40918491980847804 ) ) ;
#8658 = CARTESIAN_POINT ( 'NONE',  ( -3.458734125000000770, 1.432654583217640498, 0.9250000013655964581 ) ) ;
#8659 = DIRECTION ( 'NONE',  ( -1.000000000000000000, 0.000000000000000000, -0.000000000000000000 ) ) ;
#8660 = CARTESIAN_POINT ( 'NONE',  ( 0.000000000000000000, 9.915734732513284300, -4.762163868918174892 ) ) ;
#8661 = CARTESIAN_POINT ( 'NONE',  ( 3.458734125000001214, 1.432654583217640498, 18.00000000136560274 ) ) ;
#8662 = CARTESIAN_POINT ( 'NONE',  ( -66.55000000218494449, 8.964466094067294222, 12.49999999999996092 ) ) ;
#8663 = EDGE_CURVE ( 'NONE', #17247, #12645, #9864, .T. ) ;
#8664 = EDGE_CURVE ( 'NONE', #19956, #4420, #3643, .T. ) ;
#8665 = VERTEX_POINT ( 'NONE', #16359 ) ;
#8666 = CARTESIAN_POINT ( 'NONE',  ( 45.00000000000000000, -2.399706452296378245, 55.00000000000021316 ) ) ;
#8667 = VERTEX_POINT ( 'NONE', #18612 ) ;
#8668 = CARTESIAN_POINT ( 'NONE',  ( 54.99768183416157541, 12.16943976678977535, 12.92679907967048614 ) ) ;
#8669 = CARTESIAN_POINT ( 'NONE',  ( -68.30000000109247082, 7.933012699999995476, 14.14382582708705094 ) ) ;
#8670 = CARTESIAN_POINT ( 'NONE',  ( -70.00000000000000000, 10.00000000000000000, 14.99999999999999645 ) ) ;
#8671 = CARTESIAN_POINT ( 'NONE',  ( -1.432654583217640942, -3.458734124999999882, -3.074999998634404985 ) ) ;
#8672 = ORIENTED_EDGE ( 'NONE', *, *, #21355, .T. ) ;
#8673 = CARTESIAN_POINT ( 'NONE',  ( -90.00000000000000000, 0.000000000000000000, -9.000000000000021316 ) ) ;
#8674 = ORIENTED_EDGE ( 'NONE', *, *, #6695, .F. ) ;
#8675 = CARTESIAN_POINT ( 'NONE',  ( -65.85000000109246798, 9.999999999999998224, 17.06698730000000097 ) ) ;
#8676 = VERTEX_POINT ( 'NONE', #23657 ) ;
#8677 = CARTESIAN_POINT ( 'NONE',  ( 51.40856816583843880, 13.97181229448534978, 13.27509460956196641 ) ) ;
#8678 = CARTESIAN_POINT ( 'NONE',  ( -68.25000000218494733, 11.03553390593273598, 12.49999999999999289 ) ) ;
#8679 =( BOUNDED_CURVE ( )  B_SPLINE_CURVE ( 2, ( #1443, #8662, #19769, #23611, #10714, #3494, #17991, #3601, #23487 ),
 .UNSPECIFIED., .F., .F. ) 
 B_SPLINE_CURVE_WITH_KNOTS ( ( 3, 2, 2, 2, 3 ),
 ( 0.8124999999999993339, 0.8281249999999992228, 0.8437499999999991118, 0.8593749999999991118, 0.8749999999999990008 ),
 .UNSPECIFIED. ) 
 CURVE ( )  GEOMETRIC_REPRESENTATION_ITEM ( )  RATIONAL_B_SPLINE_CURVE ( ( 1.000000000000003331, 0.9238795325112835188, 1.000000000000000000, 0.9238795325112867385, 1.000000000000000000, 0.9238795325112867385, 1.000000000000000000, 0.9238795325112916235, 0.9999999999999951150 ) ) 
 REPRESENTATION_ITEM ( '' )  );
#8680 = DIRECTION ( 'NONE',  ( 7.087422195345011518E-32, 1.000000000000000000, -0.000000000000000000 ) ) ;
#8681 = DIRECTION ( 'NONE',  ( 1.000000000000000000, 0.000000000000000000, -4.093947403305266636E-14 ) ) ;
#8682 = CARTESIAN_POINT ( 'NONE',  ( -3.458734124999999437, 0.000000000000000000, 15.68750000136560629 ) ) ;
#8683 = CARTESIAN_POINT ( 'NONE',  ( 9.920644283265380691E-16, 4.000000000000000000, 10.87500000273119660 ) ) ;
#8684 = CARTESIAN_POINT ( 'NONE',  ( 57.75000000000000000, 7.878679656440361612, 17.12132034355964549 ) ) ;
#8685 = CARTESIAN_POINT ( 'NONE',  ( 4.999999999999999112, 6.772677083992466152, -5.538577986808826736 ) ) ;
#8686 = CARTESIAN_POINT ( 'NONE',  ( 51.12731816583844591, 12.16943976678978601, 17.07320092032949432 ) ) ;
#8687 = CARTESIAN_POINT ( 'NONE',  ( 3.458734125000000770, 1.432654583217640498, 2.550000001365598123 ) ) ;
#8688 = CARTESIAN_POINT ( 'NONE',  ( 9.920644283265380691E-16, 4.000000000000000000, 18.87500000273119838 ) ) ;
#8689 = EDGE_CURVE ( 'NONE', #12712, #10456, #22065, .T. ) ;
#8690 = CARTESIAN_POINT ( 'NONE',  ( 4.999999999999999112, 0.000000000000000000, 0.000000000000000000 ) ) ;
#8691 = EDGE_CURVE ( 'NONE', #11492, #4376, #17972, .T. ) ;
#8692 = ORIENTED_EDGE ( 'NONE', *, *, #21456, .F. ) ;
#8693 = CARTESIAN_POINT ( 'NONE',  ( 1.025207404391860050E-15, 3.458734125000000770, 10.43750000136560629 ) ) ;
#8694 = DIRECTION ( 'NONE',  ( -0.000000000000000000, -1.000000000000000000, 0.000000000000000000 ) ) ;
#8695 = ORIENTED_EDGE ( 'NONE', *, *, #13673, .F. ) ;
#8696 = DIRECTION ( 'NONE',  ( -7.703719777548925896E-32, -0.9396926207859083169, -0.3420201433256691015 ) ) ;
#8697 = CARTESIAN_POINT ( 'NONE',  ( -2.449293598294706907E-16, 4.000000000000000000, 0.1750000027311865991 ) ) ;
#8698 = DIRECTION ( 'NONE',  ( -7.087422195345011518E-32, -1.000000000000000000, -0.000000000000000000 ) ) ;
#8699 = ORIENTED_EDGE ( 'NONE', *, *, #310, .F. ) ;
#8700 = ORIENTED_EDGE ( 'NONE', *, *, #19710, .F. ) ;
#8701 = CARTESIAN_POINT ( 'NONE',  ( 4.999999999999999112, 9.915734732513284300, -4.762163868918172227 ) ) ;
#8702 = AXIS2_PLACEMENT_3D ( 'NONE', #9288, #14802, #2186 ) ;
#8703 = DIRECTION ( 'NONE',  ( 1.000000000000000000, 0.000000000000000000, 0.000000000000000000 ) ) ;
#8704 = EDGE_LOOP ( 'NONE', ( #3833, #18767, #13002, #23674 ) ) ;
#8705 = DIRECTION ( 'NONE',  ( 1.000000000000000000, 0.000000000000000000, -0.000000000000000000 ) ) ;
#8706 = LINE ( 'NONE', #15464, #13693 ) ;
#8707 = CARTESIAN_POINT ( 'NONE',  ( -3.847601380332740018, -11.25000000000000355, 5.000000000000079936 ) ) ;
#8708 = AXIS2_PLACEMENT_3D ( 'NONE', #22124, #13071, #20327 ) ;
#8709 = AXIS2_PLACEMENT_3D ( 'NONE', #13694, #23009, #10463 ) ;
#8710 = CARTESIAN_POINT ( 'NONE',  ( 66.55000000109247082, 11.46158073645647235, 16.46158073645647235 ) ) ;
#8711 = DIRECTION ( 'NONE',  ( 0.000000000000000000, 0.000000000000000000, 1.000000000000000000 ) ) ;
#8712 = CARTESIAN_POINT ( 'NONE',  ( 69.75000000218496155, 8.964466094067244484, 12.50000000000000711 ) ) ;
#8713 = CARTESIAN_POINT ( 'NONE',  ( 52.96875000000000000, 5.999999999999987566, 13.34314575050763452 ) ) ;
#8714 = CARTESIAN_POINT ( 'NONE',  ( 3.458734125000000770, -1.432654583217639610, 2.175000001365597679 ) ) ;
#8715 = CARTESIAN_POINT ( 'NONE',  ( -3.458734124999998105, -1.432654583217642275, 15.50000000136560807 ) ) ;
#8716 = CARTESIAN_POINT ( 'NONE',  ( 67.90000000218495302, 8.232233047033627571, 16.76776695296636532 ) ) ;
#8717 = DIRECTION ( 'NONE',  ( 0.000000000000000000, 0.000000000000000000, 1.000000000000000000 ) ) ;
#8718 = ORIENTED_EDGE ( 'NONE', *, *, #19021, .T. ) ;
#8719 = CARTESIAN_POINT ( 'NONE',  ( -3.058823393344586528, 2.118763015513301262, 2.039999999999997815 ) ) ;
#8720 = DIRECTION ( 'NONE',  ( 0.000000000000000000, 0.000000000000000000, 1.000000000000000000 ) ) ;
#8721 = CARTESIAN_POINT ( 'NONE',  ( -20.00005080000000035, 0.000000000000000000, 0.000000000000000000 ) ) ;
#8722 = AXIS2_PLACEMENT_3D ( 'NONE', #6428, #20665, #7996 ) ;
#8723 = AXIS2_PLACEMENT_3D ( 'NONE', #20666, #16860, #794 ) ;
#8724 = ORIENTED_EDGE ( 'NONE', *, *, #9943, .T. ) ;
#8725 = CARTESIAN_POINT ( 'NONE',  ( 45.00000000000000000, 7.098169556225943033, 56.71010071662853136 ) ) ;
#8726 = CARTESIAN_POINT ( 'NONE',  ( -67.39999999999999147, 11.76776695296636888, 13.23223304703362579 ) ) ;
#8727 = CARTESIAN_POINT ( 'NONE',  ( 59.25000000000000711, 7.171572875253819923, 17.82842712474619873 ) ) ;
#8728 = VERTEX_POINT ( 'NONE', #20154 ) ;
#8729 = LINE ( 'NONE', #15699, #8763 ) ;
#8730 = ORIENTED_EDGE ( 'NONE', *, *, #11102, .F. ) ;
#8731 = ADVANCED_FACE ( 'NONE', ( #9068 ), #14458, .T. ) ;
#8732 = CARTESIAN_POINT ( 'NONE',  ( 57.59606816583843880, 11.58880310854672935, 10.97181229448534445 ) ) ;
#8733 = CARTESIAN_POINT ( 'NONE',  ( 68.35000000218495586, 12.50000000000000000, 13.96446609406725869 ) ) ;
#8734 = CIRCLE ( 'NONE', #670, 6.000000000000000888 ) ;
#8735 = DIRECTION ( 'NONE',  ( 0.000000000000000000, 0.000000000000000000, 1.000000000000000000 ) ) ;
#8736 = CARTESIAN_POINT ( 'NONE',  ( 2.499999999999999556, 10.90201369670498721, -1.464956435139581403 ) ) ;
#8737 = CARTESIAN_POINT ( 'NONE',  ( -2.000000000000001776, 0.000000000000000000, -8.073750000000021743 ) ) ;
#8738 = VERTEX_POINT ( 'NONE', #20282 ) ;
#8739 = CIRCLE ( 'NONE', #20177, 9.000000000000000000 ) ;
#8740 = MECHANICAL_DESIGN_GEOMETRIC_PRESENTATION_REPRESENTATION (  '', ( #9898 ), #19816 ) ;
#8741 = CARTESIAN_POINT ( 'NONE',  ( -69.00000000218494733, 9.999999999999998224, 12.49999999999999289 ) ) ;
#8742 =( GEOMETRIC_REPRESENTATION_CONTEXT ( 3 ) GLOBAL_UNCERTAINTY_ASSIGNED_CONTEXT ( ( #4030 ) ) GLOBAL_UNIT_ASSIGNED_CONTEXT ( ( #9057, #5441, #20143 ) ) REPRESENTATION_CONTEXT ( 'NONE', 'WORKASPACE' ) );
#8743 = DIRECTION ( 'NONE',  ( -1.000000000000000000, 0.000000000000000000, 0.000000000000000000 ) ) ;
#8744 = CARTESIAN_POINT ( 'NONE',  ( 66.35000000109246798, 11.46158073645647235, 13.53841926354352232 ) ) ;
#8745 = CARTESIAN_POINT ( 'NONE',  ( 3.458734125000001658, 4.235727675282972223E-16, 18.18750000136560274 ) ) ;
#8746 = DIRECTION ( 'NONE',  ( 1.000000000000000000, 7.703719777548943412E-32, 0.000000000000000000 ) ) ;
#8747 = LINE ( 'NONE', #12357, #19175 ) ;
#8748 = VERTEX_POINT ( 'NONE', #18146 ) ;
#8749 = CARTESIAN_POINT ( 'NONE',  ( -3.381512639161500466, 0.7267833367865139671, -3.295601554149589330 ) ) ;
#8750 = CARTESIAN_POINT ( 'NONE',  ( 56.15625000000001421, 7.000000000000002665, 16.24264068711929099 ) ) ;
#8751 = CARTESIAN_POINT ( 'NONE',  ( -3.999999999999999112, 1.656854249492380582, 11.06250000273119660 ) ) ;
#8752 = CARTESIAN_POINT ( 'NONE',  ( 4.999999999999999112, 0.000000000000000000, 0.000000000000000000 ) ) ;
#8753 = ORIENTED_EDGE ( 'NONE', *, *, #1468, .F. ) ;
#8754 = VECTOR ( 'NONE', #8868, 1000.000000000000000 ) ;
#8755 = CARTESIAN_POINT ( 'NONE',  ( -2.366436158131400969E-16, 3.864683531250000303, -3.028124999658599048 ) ) ;
#8756 = CARTESIAN_POINT ( 'NONE',  ( 1.432654583217642275, -3.458734124999999437, -0.9499999986344030978 ) ) ;
#8757 = DIRECTION ( 'NONE',  ( 1.000000000000000000, 7.703719777548943412E-32, 0.000000000000000000 ) ) ;
#8758 = ORIENTED_EDGE ( 'NONE', *, *, #4797, .F. ) ;
#8759 = CARTESIAN_POINT ( 'NONE',  ( -4.154094228333456762, 2.398367420968013253, -3.721909803043220055 ) ) ;
#8760 = ORIENTED_EDGE ( 'NONE', *, *, #19578, .F. ) ;
#8761 = ADVANCED_FACE ( 'NONE', ( #21724 ), #14586, .T. ) ;
#8762 = CARTESIAN_POINT ( 'NONE',  ( 2.000000000000001776, 9.887492094615969966E-16, 8.073750000000021743 ) ) ;
#8763 = VECTOR ( 'NONE', #12454, 1000.000000000000114 ) ;
#8764 = EDGE_CURVE ( 'NONE', #20917, #12579, #3884, .T. ) ;
#8765 = EDGE_LOOP ( 'NONE', ( #9972, #2864, #250, #5350 ) ) ;
#8766 = CARTESIAN_POINT ( 'NONE',  ( -3.999999999999998224, -1.656854249492383246, 18.06250000000001421 ) ) ;
#8767 = CARTESIAN_POINT ( 'NONE',  ( -66.49999999999998579, 9.999999999999998224, 12.49999999999999289 ) ) ;
#8768 = CARTESIAN_POINT ( 'NONE',  ( -65.65000000109247935, 9.999999999999998224, 17.06698730000000097 ) ) ;
#8769 = SURFACE_SIDE_STYLE ('',( #16075 ) ) ;
#8770 = AXIS2_PLACEMENT_3D ( 'NONE', #8045, #20706, #11649 ) ;
#8771 = EDGE_CURVE ( 'NONE', #19381, #9225, #12787, .T. ) ;
#8772 = LINE ( 'NONE', #19759, #14453 ) ;
#8773 = AXIS2_PLACEMENT_3D ( 'NONE', #1586, #10380, #3272 ) ;
#8774 = CARTESIAN_POINT ( 'NONE',  ( -70.70000000000000284, 12.50000000000000000, 14.99999999999999645 ) ) ;
#8775 = CARTESIAN_POINT ( 'NONE',  ( -65.00000000000000000, -9.999999999999998224, 20.00000000000001421 ) ) ;
#8776 = CARTESIAN_POINT ( 'NONE',  ( 60.00000000000001421, 13.93055609735682054, 14.31316200167426267 ) ) ;
#8777 = AXIS2_PLACEMENT_3D ( 'NONE', #13516, #2226, #13402 ) ;
#8778 = CARTESIAN_POINT ( 'NONE',  ( -1.432654583217640498, 3.458734125000000770, -2.199999998634404541 ) ) ;
#8779 = DIRECTION ( 'NONE',  ( -1.000000000000000000, 0.000000000000000000, -0.000000000000000000 ) ) ;
#8780 = CARTESIAN_POINT ( 'NONE',  ( 15.00195451966726523, -11.25000000000000355, 5.000000000000079936 ) ) ;
#8781 = CARTESIAN_POINT ( 'NONE',  ( 9.920644283265380691E-16, 4.000000000000000000, 9.875000002731196602 ) ) ;
#8782 = CARTESIAN_POINT ( 'NONE',  ( 0.000000000000000000, 5.538577986808997267, -6.772677083992326708 ) ) ;
#8783 = ORIENTED_EDGE ( 'NONE', *, *, #7862, .T. ) ;
#8784 = CARTESIAN_POINT ( 'NONE',  ( -71.15000000109247935, 11.46158073645647235, 16.46158073645647235 ) ) ;
#8785 = VERTEX_POINT ( 'NONE', #16477 ) ;
#8786 = CARTESIAN_POINT ( 'NONE',  ( 54.06018183416157541, 7.000000000000000000, 14.93194885905437097 ) ) ;
#8787 = CARTESIAN_POINT ( 'NONE',  ( -67.00000000109247367, 12.06698730000000275, 14.14382582708705094 ) ) ;
#8788 = AXIS2_PLACEMENT_3D ( 'NONE', #3809, #18529, #5731 ) ;
#8789 = DIRECTION ( 'NONE',  ( 1.000000000000000000, 0.000000000000000000, 0.000000000000000000 ) ) ;
#8790 = ADVANCED_BREP_SHAPE_REPRESENTATION ( '', ( #6915, #7318 ), #9900 ) ;
#8791 = ADVANCED_FACE ( 'NONE', ( #10871 ), #7500, .T. ) ;
#8792 = VECTOR ( 'NONE', #14011, 1000.000000000000000 ) ;
#8793 = CARTESIAN_POINT ( 'NONE',  ( 1.432654583217642053, -3.458734124999999437, -1.949999998634404097 ) ) ;
#8794 = ORIENTED_EDGE ( 'NONE', *, *, #10412, .T. ) ;
#8795 = DIRECTION ( 'NONE',  ( 1.000000000000000000, 0.000000000000000000, 0.000000000000000000 ) ) ;
#8796 = AXIS2_PLACEMENT_3D ( 'NONE', #8007, #2238, #4041 ) ;
#8797 = EDGE_CURVE ( 'NONE', #1835, #6127, #56, .T. ) ;
#8798 = EDGE_CURVE ( 'NONE', #10010, #2729, #14698, .T. ) ;
#8799 = ORIENTED_EDGE ( 'NONE', *, *, #13381, .F. ) ;
#8800 = DIRECTION ( 'NONE',  ( 0.000000000000000000, 0.000000000000000000, -1.000000000000000000 ) ) ;
#8801 = ORIENTED_EDGE ( 'NONE', *, *, #22768, .T. ) ;
#8802 = CARTESIAN_POINT ( 'NONE',  ( 50.65856816583843880, 7.028187705514647554, 16.31069182806492179 ) ) ;
#8803 = AXIS2_PLACEMENT_3D ( 'NONE', #16093, #6983, #1574 ) ;
#8804 = CARTESIAN_POINT ( 'NONE',  ( -68.10000000218495586, 8.232233047033629347, 13.23223304703362402 ) ) ;
#8805 = VECTOR ( 'NONE', #13237, 1000.000000000000000 ) ;
#8806 = EDGE_CURVE ( 'NONE', #4502, #19518, #11100, .T. ) ;
#8807 = DIRECTION ( 'NONE',  ( 1.000000000000000000, -0.000000000000000000, -0.000000000000000000 ) ) ;
#8808 = EDGE_CURVE ( 'NONE', #9681, #5198, #5683, .T. ) ;
#8809 = CARTESIAN_POINT ( 'NONE',  ( 31.52885079676620705, -9.000000000000005329, 5.000000000000079936 ) ) ;
#8810 = CARTESIAN_POINT ( 'NONE',  ( 3.458734125000001658, 4.235727675282972223E-16, 14.18750000136560629 ) ) ;
#8811 = CARTESIAN_POINT ( 'NONE',  ( -1.656854249492379250, 4.000000000000000000, 9.937500002731198379 ) ) ;
#8812 = CARTESIAN_POINT ( 'NONE',  ( 59.62500000000000711, 12.12132034355964727, 17.12132034355963484 ) ) ;
#8813 = DIRECTION ( 'NONE',  ( -1.000000000000000000, 0.000000000000000000, 0.000000000000000000 ) ) ;
#8814 = CIRCLE ( 'NONE', #2664, 8.749000000000004107 ) ;
#8815 = CARTESIAN_POINT ( 'NONE',  ( 56.90625000000000711, 12.99999999999999645, 13.75735931288070191 ) ) ;
#8816 = CARTESIAN_POINT ( 'NONE',  ( -2.445694354108819635, -2.445694354108820967, 3.112500001365597679 ) ) ;
#8817 = CARTESIAN_POINT ( 'NONE',  ( 0.01183343685760930748, -3.466145975376039079, 2.040000000000000036 ) ) ;
#8818 = CARTESIAN_POINT ( 'NONE',  ( -68.39999999999999147, 11.76776695296636888, 16.76776695296636532 ) ) ;
#8819 = CIRCLE ( 'NONE', #11887, 4.000000000000000000 ) ;
#8820 = ORIENTED_EDGE ( 'NONE', *, *, #12356, .T. ) ;
#8821 = DIRECTION ( 'NONE',  ( -0.000000000000000000, 0.000000000000000000, -1.000000000000000000 ) ) ;
#8822 = CARTESIAN_POINT ( 'NONE',  ( -2.742827927723112236, -3.035229711105190464, -3.433252694550595230 ) ) ;
#8823 = EDGE_LOOP ( 'NONE', ( #18823, #17003, #10751, #6744, #21091 ) ) ;
#8824 = CARTESIAN_POINT ( 'NONE',  ( 59.06250000000000711, 6.999999999999997335, 15.00000000000000533 ) ) ;
#8825 = VECTOR ( 'NONE', #10236, 1000.000000000000000 ) ;
#8826 = CARTESIAN_POINT ( 'NONE',  ( 4.000000000000000000, 4.898587196589412829E-16, -0.07499999726881187434 ) ) ;
#8827 = FACE_OUTER_BOUND ( 'NONE', #16463, .T. ) ;
#8828 = VERTEX_POINT ( 'NONE', #18494 ) ;
#8829 = CARTESIAN_POINT ( 'NONE',  ( 4.000000000000000888, 4.898587196589412829E-16, 17.50000000000001066 ) ) ;
#8830 = ORIENTED_EDGE ( 'NONE', *, *, #2346, .F. ) ;
#8831 = CARTESIAN_POINT ( 'NONE',  ( 4.332341089154587834E-16, 7.505553499465137612, -3.700000000000000178 ) ) ;
#8832 =( BOUNDED_CURVE ( )  B_SPLINE_CURVE ( 2, ( #13708, #2538, #756, #4590, #20969, #11925, #3497, #15964, #23021 ),
 .UNSPECIFIED., .F., .F. ) 
 B_SPLINE_CURVE_WITH_KNOTS ( ( 3, 2, 2, 2, 3 ),
 ( 0.2000000000000000111, 0.2124999999999999944, 0.2250000000000000056, 0.2374999999999999889, 0.2500000000000000000 ),
 .UNSPECIFIED. ) 
 CURVE ( )  GEOMETRIC_REPRESENTATION_ITEM ( )  RATIONAL_B_SPLINE_CURVE ( ( 1.000000000000000000, 0.9238795325112867385, 1.000000000000000000, 0.9238795325112867385, 1.000000000000000000, 0.9238795325112867385, 1.000000000000000000, 0.9238795325112867385, 1.000000000000000000 ) ) 
 REPRESENTATION_ITEM ( '' )  );
#8833 = ADVANCED_FACE ( 'NONE', ( #9417 ), #16707, .T. ) ;
#8834 = CARTESIAN_POINT ( 'NONE',  ( -66.74999999999998579, 12.50000000000000000, 16.03553390593273775 ) ) ;
#8835 = ORIENTED_EDGE ( 'NONE', *, *, #1266, .F. ) ;
#8836 = CARTESIAN_POINT ( 'NONE',  ( 3.540020015735602765, 2.810662092924382627, -3.602146406945867962 ) ) ;
#8837 = CARTESIAN_POINT ( 'NONE',  ( -1.656854249492380138, -3.999999999999999112, 12.18750000000001066 ) ) ;
#8838 = EDGE_CURVE ( 'NONE', #5980, #12663, #1406, .T. ) ;
#8839 = ORIENTED_EDGE ( 'NONE', *, *, #14508, .T. ) ;
#8840 = CARTESIAN_POINT ( 'NONE',  ( 4.000000000000000000, 0.9868501483902631932, -0.09357334158579604100 ) ) ;
#8841 = ADVANCED_FACE ( 'NONE', ( #17309 ), #15689, .F. ) ;
#8842 = AXIS2_PLACEMENT_3D ( 'NONE', #20830, #15482, #22753 ) ;
#8843 = CARTESIAN_POINT ( 'NONE',  ( 70.95000000000000284, 8.964466094067258695, 17.50000000000000355 ) ) ;
#8844 = CARTESIAN_POINT ( 'NONE',  ( 1.656854249492384135, -3.999999999999999112, 17.43750000273119483 ) ) ;
#8845 = DIRECTION ( 'NONE',  ( -0.000000000000000000, -0.000000000000000000, 1.000000000000000000 ) ) ;
#8846 = CARTESIAN_POINT ( 'NONE',  ( 58.34606816583844591, 8.411196891453267099, 19.02818770551464667 ) ) ;
#8847 = DIRECTION ( 'NONE',  ( 0.000000000000000000, -1.000000000000000000, 0.000000000000000000 ) ) ;
#8848 = CARTESIAN_POINT ( 'NONE',  ( -1.432654583217639610, -3.458734124999999882, 16.62500000136560629 ) ) ;
#8849 = DIRECTION ( 'NONE',  ( 0.000000000000000000, 0.8660254037844380415, -0.5000000000000009992 ) ) ;
#8850 = DIRECTION ( 'NONE',  ( 0.000000000000000000, -1.000000000000000000, 0.000000000000000000 ) ) ;
#8851 = ORIENTED_EDGE ( 'NONE', *, *, #23627, .T. ) ;
#8852 = CARTESIAN_POINT ( 'NONE',  ( -1.520000000000000462, 0.000000000000000000, 0.000000000000000000 ) ) ;
#8853 = LINE ( 'NONE', #16264, #23550 ) ;
#8854 = DIRECTION ( 'NONE',  ( 1.000000000000000000, 0.000000000000000000, 0.000000000000000000 ) ) ;
#8855 = CIRCLE ( 'NONE', #22197, 4.000000000000000888 ) ;
#8856 = ORIENTED_EDGE ( 'NONE', *, *, #10982, .T. ) ;
#8857 = CARTESIAN_POINT ( 'NONE',  ( -10.13078668033273999, -11.25000000000000355, 5.000000000000079936 ) ) ;
#8858 = CARTESIAN_POINT ( 'NONE',  ( -1.489200000000000301, 1.009010990753487416E-15, 8.239200000000002078 ) ) ;
#8859 = ORIENTED_EDGE ( 'NONE', *, *, #4571, .F. ) ;
#8860 = CARTESIAN_POINT ( 'NONE',  ( 65.95000000218495018, 12.50000000000000000, 13.96446609406725692 ) ) ;
#8861 = ORIENTED_EDGE ( 'NONE', *, *, #9103, .F. ) ;
#8862 = CARTESIAN_POINT ( 'NONE',  ( 53.71875000000002132, 14.00000000000000888, 16.65685424949235482 ) ) ;
#8863 = EDGE_CURVE ( 'NONE', #9892, #18376, #10026, .T. ) ;
#8864 = CARTESIAN_POINT ( 'NONE',  ( 69.05000000218494449, 11.03553390593273598, 12.49999999999999289 ) ) ;
#8865 =( BOUNDED_CURVE ( )  B_SPLINE_CURVE ( 2, ( #7572, #22149, #366, #15016, #9619, #5882, #20472, #4078, #16910 ),
 .UNSPECIFIED., .F., .F. ) 
 B_SPLINE_CURVE_WITH_KNOTS ( ( 3, 2, 2, 2, 3 ),
 ( 0.06249999999999961836, 0.07812499999999952816, 0.09374999999999943101, 0.1093749999999993339, 0.1249999999999992367 ),
 .UNSPECIFIED. ) 
 CURVE ( )  GEOMETRIC_REPRESENTATION_ITEM ( )  RATIONAL_B_SPLINE_CURVE ( ( 1.000000000000001776, 0.9238795325112848511, 1.000000000000000000, 0.9238795325112867385, 1.000000000000000000, 0.9238795325112867385, 1.000000000000000000, 0.9238795325112904022, 0.9999999999999963363 ) ) 
 REPRESENTATION_ITEM ( '' )  );
#8866 = DIRECTION ( 'NONE',  ( -1.848892746611741766E-32, -0.3420201433256689905, 0.9396926207859082059 ) ) ;
#8867 = LINE ( 'NONE', #8736, #10652 ) ;
#8868 = DIRECTION ( 'NONE',  ( -1.000000000000000000, -7.703719777548943412E-32, 0.000000000000000000 ) ) ;
#8869 = ORIENTED_EDGE ( 'NONE', *, *, #20605, .F. ) ;
#8870 = VECTOR ( 'NONE', #21770, 1000.000000000000000 ) ;
#8871 = APPLICATION_CONTEXT ( 'automotive_design' ) ;
#8872 = CARTESIAN_POINT ( 'NONE',  ( -1.600000000000004086, 0.000000000000000000, 0.000000000000000000 ) ) ;
#8873 = CARTESIAN_POINT ( 'NONE',  ( 57.34143183416159673, 8.275094609562001935, 18.97181229448536044 ) ) ;
#8874 = FACE_OUTER_BOUND ( 'NONE', #6689, .T. ) ;
#8875 = CARTESIAN_POINT ( 'NONE',  ( 66.90000000109246514, 7.933012699999995476, 14.14382582708705094 ) ) ;
#8876 = CARTESIAN_POINT ( 'NONE',  ( 1.432654583217641386, 3.458734125000000770, 17.37500000136560274 ) ) ;
#8877 = CARTESIAN_POINT ( 'NONE',  ( -69.14999999999999147, 12.50000000000000000, 16.03553390593273775 ) ) ;
#8878 = DIRECTION ( 'NONE',  ( 0.000000000000000000, -0.5877852522924801315, 0.8090169943749423442 ) ) ;
#8879 = EDGE_LOOP ( 'NONE', ( #2842, #8506, #2571, #8718 ) ) ;
#8880 = PLANE ( 'NONE',  #7413 ) ;
#8881 = CARTESIAN_POINT ( 'NONE',  ( 59.06250000000000711, 6.999999999999997335, 15.00000000000000533 ) ) ;
#8882 = CARTESIAN_POINT ( 'NONE',  ( -3.999999999999999112, 0.000000000000000000, 11.12500000273119660 ) ) ;
#8883 = ORIENTED_EDGE ( 'NONE', *, *, #8171, .T. ) ;
#8884 = CARTESIAN_POINT ( 'NONE',  ( 68.09999999999999432, 9.999999999999998224, 12.49999999999999289 ) ) ;
#8885 = CARTESIAN_POINT ( 'NONE',  ( -3.458734125000000326, 0.000000000000000000, -0.2624999986344037084 ) ) ;
#8886 = DIRECTION ( 'NONE',  ( 1.000000000000000000, 0.000000000000000000, 0.000000000000000000 ) ) ;
#8887 = ORIENTED_EDGE ( 'NONE', *, *, #19191, .F. ) ;
#8888 = CARTESIAN_POINT ( 'NONE',  ( 4.999999999999999112, 9.314797388894909602, -1.239665997526783858 ) ) ;
#8889 = VERTEX_POINT ( 'NONE', #1082 ) ;
#8890 = CARTESIAN_POINT ( 'NONE',  ( -15.56739012628458774, -7.386661945853154165, 10.00000000000008882 ) ) ;
#8891 = CARTESIAN_POINT ( 'NONE',  ( -1.656854249492380138, -3.999999999999999112, 17.18750000000001066 ) ) ;
#8892 = CARTESIAN_POINT ( 'NONE',  ( 2.500000000000000000, -1.178949249685214307, 2.042000000000001592 ) ) ;
#8893 = DIRECTION ( 'NONE',  ( 0.000000000000000000, 1.000000000000000000, -1.287488025362403787E-15 ) ) ;
#8894 = DIRECTION ( 'NONE',  ( -0.000000000000000000, -0.000000000000000000, 1.000000000000000000 ) ) ;
#8895 = CARTESIAN_POINT ( 'NONE',  ( 32.14370665323380649, -9.000000000000001776, 5.000000000000079936 ) ) ;
#8896 = CARTESIAN_POINT ( 'NONE',  ( -67.95000000000000284, 7.499999999999995559, 13.96446609406725692 ) ) ;
#8897 = CARTESIAN_POINT ( 'NONE',  ( 66.50000000218494733, 8.232233047033629347, 13.23223304703362402 ) ) ;
#8898 = CARTESIAN_POINT ( 'NONE',  ( 60.00000000000004263, 13.03655146502352480, 15.27384441607152965 ) ) ;
#8899 = DIRECTION ( 'NONE',  ( -0.000000000000000000, 0.000000000000000000, -1.000000000000000000 ) ) ;
#8900 = ADVANCED_FACE ( 'NONE', ( #4577 ), #10350, .T. ) ;
#8901 = CARTESIAN_POINT ( 'NONE',  ( 1.432654583217642275, -3.458734124999999882, -0.6999999986344028757 ) ) ;
#8902 = CARTESIAN_POINT ( 'NONE',  ( -67.70000000218493597, 11.76776695296636888, 16.76776695296636532 ) ) ;
#8903 = LINE ( 'NONE', #14540, #4689 ) ;
#8904 = CARTESIAN_POINT ( 'NONE',  ( 3.458734125000001214, 1.432654583217640498, 19.00000000136560629 ) ) ;
#8905 = CARTESIAN_POINT ( 'NONE',  ( 4.211140560182196957, 2.431303136016536470, -3.745885042887433514 ) ) ;
#8906 = B_SPLINE_CURVE_WITH_KNOTS ( 'NONE', 3,
 ( #8326, #8214, #18969, #9772, #11468, #15415 ),
 .UNSPECIFIED., .F., .F.,
 ( 4, 2, 4 ),
 ( -3.640115492409406142E-06, 0.0002066546034006526487, 0.0004169493222937146744 ),
 .UNSPECIFIED. ) ;
#8907 = EDGE_LOOP ( 'NONE', ( #16172, #10476, #6687, #20725 ) ) ;
#8908 = CARTESIAN_POINT ( 'NONE',  ( 1.656854249492384135, -3.999999999999999112, 14.43750000273119660 ) ) ;
#8909 = VERTEX_POINT ( 'NONE', #8296 ) ;
#8910 = CARTESIAN_POINT ( 'NONE',  ( 58.37268183416157541, 7.219692298483935566, 12.12345345202367675 ) ) ;
#8911 = CARTESIAN_POINT ( 'NONE',  ( -66.75000000109247367, 8.538419263543524096, 13.53841926354352054 ) ) ;
#8912 = CARTESIAN_POINT ( 'NONE',  ( -7.229187218286264707E-16, 1.417950490603859619E-15, 5.000000000000007994 ) ) ;
#8913 = ADVANCED_FACE ( 'NONE', ( #6841 ), #15618, .F. ) ;
#8914 = CARTESIAN_POINT ( 'NONE',  ( -2.445694354108819635, -2.445694354108820523, -2.137499998634403653 ) ) ;
#8915 = ORIENTED_EDGE ( 'NONE', *, *, #21597, .F. ) ;
#8916 = DIRECTION ( 'NONE',  ( 0.9396926207859107594, -0.3420201433256623291, 3.697785493223492838E-32 ) ) ;
#8917 = ORIENTED_EDGE ( 'NONE', *, *, #4528, .F. ) ;
#8918 = CIRCLE ( 'NONE', #21488, 7.000000000000000000 ) ;
#8919 = DIRECTION ( 'NONE',  ( 1.000000000000000000, -0.000000000000000000, -0.000000000000000000 ) ) ;
#8920 = ORIENTED_EDGE ( 'NONE', *, *, #7164, .F. ) ;
#8921 = AXIS2_PLACEMENT_3D ( 'NONE', #1322, #19296, #10114 ) ;
#8922 = CARTESIAN_POINT ( 'NONE',  ( 54.50231816583843170, 12.07320092032949610, 12.83056023321021044 ) ) ;
#8923 = CARTESIAN_POINT ( 'NONE',  ( -70.05000000109247082, 9.999999999999998224, 12.93301269999999192 ) ) ;
#8924 = FACE_OUTER_BOUND ( 'NONE', #7058, .T. ) ;
#8925 = DIRECTION ( 'NONE',  ( -0.000000000000000000, 0.000000000000000000, -1.000000000000000000 ) ) ;
#8926 = CARTESIAN_POINT ( 'NONE',  ( -2.445694354108818303, -2.445694354108820967, 16.81250000136560629 ) ) ;
#8927 = CARTESIAN_POINT ( 'NONE',  ( -1.656854249492381248, -3.999999999999999112, -2.387499997268812013 ) ) ;
#8928 = CARTESIAN_POINT ( 'NONE',  ( 52.78125000000000711, 8.757359312880703683, 11.99999999999999822 ) ) ;
#8929 = CYLINDRICAL_SURFACE ( 'NONE', #16739, 8.749000000000002331 ) ;
#8930 = ADVANCED_FACE ( 'NONE', ( #11911 ), #22886, .F. ) ;
#8931 = CARTESIAN_POINT ( 'NONE',  ( 51.87731816583844591, 7.830560233210212218, 12.92679907967049679 ) ) ;
#8932 = EDGE_CURVE ( 'NONE', #22668, #22906, #11787, .T. ) ;
#8933 = CARTESIAN_POINT ( 'NONE',  ( 1.432654583217640276, 3.458734125000000770, -1.324999998634403653 ) ) ;
#8934 = DIRECTION ( 'NONE',  ( -1.000000000000000000, 0.000000000000000000, 0.000000000000000000 ) ) ;
#8935 = AXIS2_PLACEMENT_3D ( 'NONE', #14891, #12973, #13207 ) ;
#8936 = CARTESIAN_POINT ( 'NONE',  ( 4.999999999999999112, 3.174628368996190719, -8.152713396088728359 ) ) ;
#8937 = VERTEX_POINT ( 'NONE', #13821 ) ;
#8938 = CARTESIAN_POINT ( 'NONE',  ( -4.000000000000000000, -1.560351142792950618, -0.2242961665059814425 ) ) ;
#8939 = CARTESIAN_POINT ( 'NONE',  ( 0.000000000000000000, -8.264486777890139635, 4.472189673936757259 ) ) ;
#8940 = ORIENTED_EDGE ( 'NONE', *, *, #14340, .F. ) ;
#8941 = CARTESIAN_POINT ( 'NONE',  ( 54.18750000000000711, 9.999999999999989342, 11.99999999999999467 ) ) ;
#8942 = SURFACE_STYLE_FILL_AREA ( #18026 ) ;
#8943 = CARTESIAN_POINT ( 'NONE',  ( 4.000000000000000000, 4.898587196589412829E-16, -1.074999997268812679 ) ) ;
#8944 = VECTOR ( 'NONE', #22993, 1000.000000000000000 ) ;
#8945 = EDGE_CURVE ( 'NONE', #6808, #17107, #2763, .T. ) ;
#8946 = CARTESIAN_POINT ( 'NONE',  ( -9.302608809283439584, -8.974600000000002353, 5.000000000000079936 ) ) ;
#8947 = ORIENTED_EDGE ( 'NONE', *, *, #1468, .T. ) ;
#8948 = EDGE_CURVE ( 'NONE', #3346, #2006, #10245, .T. ) ;
#8949 = CARTESIAN_POINT ( 'NONE',  ( -3.999999999999999112, 0.000000000000000000, 17.00000000000001066 ) ) ;
#8950 = EDGE_LOOP ( 'NONE', ( #18629, #22250, #12427, #1069 ) ) ;
#8951 = CARTESIAN_POINT ( 'NONE',  ( 4.999999999999999112, 6.478011392632890164, 6.807171995660607600 ) ) ;
#8952 = DIRECTION ( 'NONE',  ( -1.000000000000000000, -0.000000000000000000, -0.000000000000000000 ) ) ;
#8953 = ORIENTED_EDGE ( 'NONE', *, *, #13250, .T. ) ;
#8954 = LINE ( 'NONE', #12895, #349 ) ;
#8955 = CARTESIAN_POINT ( 'NONE',  ( -3.999999999999998224, -1.656854249492383246, 11.06250000000001066 ) ) ;
#8956 = EDGE_LOOP ( 'NONE', ( #7261, #6086 ) ) ;
#8957 = DIRECTION ( 'NONE',  ( -1.000000000000000000, 0.000000000000000000, 0.000000000000000000 ) ) ;
#8958 = CARTESIAN_POINT ( 'NONE',  ( 72.25000000000000000, 12.50000000000000000, 13.96446609406725869 ) ) ;
#8959 = AXIS2_PLACEMENT_3D ( 'NONE', #12829, #5497, #3816 ) ;
#8960 = EDGE_CURVE ( 'NONE', #15223, #6641, #4686, .T. ) ;
#8961 = CARTESIAN_POINT ( 'NONE',  ( 37.14043617343693171, 11.79741794011847311, 10.00000000000008882 ) ) ;
#8962 = CARTESIAN_POINT ( 'NONE',  ( -6.499999999999999112, 7.960204194457795477E-16, 2.040000000000001812 ) ) ;
#8963 = CARTESIAN_POINT ( 'NONE',  ( 52.12500000000000711, 12.82842712474620228, 17.82842712474617386 ) ) ;
#8964 = EDGE_CURVE ( 'NONE', #13557, #2919, #21427, .T. ) ;
#8965 = CARTESIAN_POINT ( 'NONE',  ( 2.445694354108820079, 2.445694354108820523, -0.6374999986344040970 ) ) ;
#8966 = SURFACE_STYLE_USAGE ( .BOTH. , #5461 ) ;
#8967 = CARTESIAN_POINT ( 'NONE',  ( -3.458734124999998105, -1.432654583217642275, 13.50000000136560452 ) ) ;
#8968 = CARTESIAN_POINT ( 'NONE',  ( -4.000000000000000888, 1.656854249492380582, 0.2375000000000018763 ) ) ;
#8969 = CLOSED_SHELL ( 'NONE', ( #6289, #1675, #1582, #14220, #14231, #416, #11540, #14640, #19845, #22597, #19912, #3561, #6020, #12321, #22045, #8791, #7642, #6334, #20504, #16103, #21951, #5973, #10168, #2141, #16925, #11251, #10699, #10264, #1569, #5429, #5117, #10677, #10984, #8396, #21026, #17577, #21956, #5254, #13968, #12218, #17310, #22497, #13479, #20499, #15672, #3800, #15169, #17477, #9073, #8499 ) ) ;
#8970 = CARTESIAN_POINT ( 'NONE',  ( -70.30000000218494449, 8.232233047033627571, 16.76776695296636532 ) ) ;
#8971 = ORIENTED_EDGE ( 'NONE', *, *, #7093, .T. ) ;
#8972 = DIRECTION ( 'NONE',  ( 0.000000000000000000, 0.000000000000000000, -1.000000000000000000 ) ) ;
#8973 =( BOUNDED_SURFACE ( )  B_SPLINE_SURFACE ( 1, 2, ( 
 ( #6583, #9831, #19368, #22850, #2612, #8154, #17124, #822, #1169, #11989, #21268, #22977, #17364, #2733, #6465, #9956, #15812, #15465, #13787, #10315, #15353, #8509, #932, #20922, #19258, #4540, #22620, #8268, #10193, #4771, #21155, #22736, #12226, #23084, #6347, #4656, #13897, #2962, #17484, #17604, #13660, #1050, #4891, #19495, #11877, #9096, #10897, #23447, #23568, #21635, #7303, #12344, #16276, #1758, #7175, #8864, #16389, #1392, #16041, #8987, #18177, #8617, #19725, #17716, #3451, #23686, #12813, #21398, #10552, #8733, #14610, #21872, #6810, #3322, #10667, #7052, #5124, #1278, #16160, #1525, #5478, #14373, #3092, #5239, #17826, #15919, #23197, #12461, #5015, #10435, #17943, #14132, #12583, #14490, #19606, #6940, #23331, #19843, #5365, #21753, #10788, #18063, #14255, #21513, #12708, #1643, #19960, #3204, #3562, #552, #16619, #2230, #22340, #81, #3909, #4152, #11245, #5835, #13161, #20072, #14724, #7767, #22459, #11367, #3672, #20423, #15196, #4033, #14973 ),
 ( #18644, #11008, #2353, #9442, #11135, #7415, #18291, #18410, #21985, #1874, #9222, #9573, #5599, #16737, #16867, #20308, #9327, #442, #5955, #5717, #13051, #15086, #12925, #22224, #13279, #16504, #9684, #318, #1988, #20186, #3795, #198, #7528, #14844, #22098, #20548, #18519, #7652, #11499, #2106, #18772, #16978, #7878, #6071, #22706, #8358, #17093, #8241, #23058, #22950, #13404, #8485, #4632, #10286, #17574, #9802, #12078, #19120, #22820, #20671, #18880, #13518, #4276, #20784, #15325, #17222, #2463, #798, #15561, #11966, #8001, #11610, #17338, #8129, #6435, #1023, #19345, #15674, #667, #2581, #19232, #6558, #11843, #13633, #22595, #10050, #905, #2822, #13874, #6199, #10166, #4388, #11729, #18993, #9925, #6316, #17461, #15439, #21131, #2708, #20894, #4508, #13753, #21015, #4746, #2935, #1141, #15788, #14229, #16013, #3299, #15896, #12681, #6783, #12432, #7148, #12198, #21727, #23301, #17800, #16137, #1371, #4861, #21484, #7025, #1615, #10873, #1729, #4989 ) ),
 .UNSPECIFIED., .F., .F., .F. ) 
 B_SPLINE_SURFACE_WITH_KNOTS ( ( 2, 2 ),
 ( 3, 2, 2, 2, 2, 2, 2, 2, 2, 2, 2, 2, 2, 2, 2, 2, 2, 2, 2, 2, 2, 2, 2, 2, 2, 2, 2, 2, 2, 2, 2, 2, 2, 2, 2, 2, 2, 2, 2, 2, 2, 2, 2, 2, 2, 2, 2, 2, 2, 2, 2, 2, 2, 2, 2, 2, 2, 2, 2, 2, 2, 2, 2, 2, 3 ),
 ( 0.000000000000000000, 1.000000000000000000 ),
 ( 0.000000000000000000, 0.01562500000000000000, 0.03125000000000000000, 0.04687500000000000000, 0.06250000000000000000, 0.07812500000000000000, 0.09375000000000000000, 0.1093750000000000000, 0.1250000000000000000, 0.1406250000000000000, 0.1562500000000000000, 0.1718750000000000000, 0.1875000000000000000, 0.2031250000000000000, 0.2187500000000000000, 0.2343750000000000000, 0.2500000000000000000, 0.2656250000000000000, 0.2812500000000000000, 0.2968750000000000000, 0.3125000000000000000, 0.3281250000000000000, 0.3437500000000000000, 0.3593750000000000000, 0.3750000000000000000, 0.3906250000000000000, 0.4062500000000000000, 0.4218750000000000000, 0.4375000000000000000, 0.4531250000000000000, 0.4687500000000000000, 0.4843750000000000000, 0.5000000000000000000, 0.5156250000000000000, 0.5312500000000000000, 0.5468750000000000000, 0.5625000000000000000, 0.5781250000000000000, 0.5937500000000000000, 0.6093750000000000000, 0.6250000000000000000, 0.6406250000000000000, 0.6562500000000000000, 0.6718750000000000000, 0.6875000000000000000, 0.7031250000000000000, 0.7187500000000000000, 0.7343750000000000000, 0.7500000000000000000, 0.7656250000000000000, 0.7812500000000000000, 0.7968750000000000000, 0.8125000000000000000, 0.8281250000000000000, 0.8437500000000000000, 0.8593750000000000000, 0.8750000000000000000, 0.8906250000000000000, 0.9062500000000000000, 0.9218750000000000000, 0.9375000000000000000, 0.9531250000000000000, 0.9687500000000000000, 0.9843750000000000000, 1.000000000000000000 ),
 .UNSPECIFIED. ) 
 GEOMETRIC_REPRESENTATION_ITEM ( )  RATIONAL_B_SPLINE_SURFACE ( (
 ( 1.000000000000000000, 0.9238795325112867385, 1.000000000000000000, 0.9238795325112867385, 1.000000000000000000, 0.9238795325112867385, 1.000000000000000000, 0.9238795325112867385, 1.000000000000000000, 0.9238795325112867385, 1.000000000000000000, 0.9238795325112867385, 1.000000000000000000, 0.9238795325112867385, 1.000000000000000000, 0.9238795325112867385, 1.000000000000000000, 0.9238795325112867385, 1.000000000000000000, 0.9238795325112867385, 1.000000000000000000, 0.9238795325112867385, 1.000000000000000000, 0.9238795325112867385, 1.000000000000000000, 0.9238795325112867385, 1.000000000000000000, 0.9238795325112867385, 1.000000000000000000, 0.9238795325112867385, 1.000000000000000000, 0.9238795325112867385, 1.000000000000000000, 0.9238795325112867385, 1.000000000000000000, 0.9238795325112867385, 1.000000000000000000, 0.9238795325112867385, 1.000000000000000000, 0.9238795325112867385, 1.000000000000000000, 0.9238795325112867385, 1.000000000000000000, 0.9238795325112867385, 1.000000000000000000, 0.9238795325112867385, 1.000000000000000000, 0.9238795325112867385, 1.000000000000000000, 0.9238795325112867385, 1.000000000000000000, 0.9238795325112867385, 1.000000000000000000, 0.9238795325112867385, 1.000000000000000000, 0.9238795325112867385, 1.000000000000000000, 0.9238795325112867385, 1.000000000000000000, 0.9238795325112867385, 1.000000000000000000, 0.9238795325112867385, 1.000000000000000000, 0.9238795325112867385, 1.000000000000000000, 0.9238795325112867385, 1.000000000000000000, 0.9238795325112867385, 1.000000000000000000, 0.9238795325112867385, 1.000000000000000000, 0.9238795325112867385, 1.000000000000000000, 0.9238795325112867385, 1.000000000000000000, 0.9238795325112867385, 1.000000000000000000, 0.9238795325112867385, 1.000000000000000000, 0.9238795325112867385, 1.000000000000000000, 0.9238795325112867385, 1.000000000000000000, 0.9238795325112867385, 1.000000000000000000, 0.9238795325112867385, 1.000000000000000000, 0.9238795325112867385, 1.000000000000000000, 0.9238795325112867385, 1.000000000000000000, 0.9238795325112867385, 1.000000000000000000, 0.9238795325112867385, 1.000000000000000000, 0.9238795325112867385, 1.000000000000000000, 0.9238795325112867385, 1.000000000000000000, 0.9238795325112867385, 1.000000000000000000, 0.9238795325112867385, 1.000000000000000000, 0.9238795325112867385, 1.000000000000000000, 0.9238795325112867385, 1.000000000000000000, 0.9238795325112867385, 1.000000000000000000, 0.9238795325112867385, 1.000000000000000000, 0.9238795325112867385, 1.000000000000000000, 0.9238795325112867385, 1.000000000000000000, 0.9238795325112867385, 1.000000000000000000, 0.9238795325112867385, 1.000000000000000000, 0.9238795325112867385, 1.000000000000000000, 0.9238795325112867385, 1.000000000000000000, 0.9238795325112867385, 1.000000000000000000, 0.9238795325112867385, 1.000000000000000000, 0.9238795325112867385, 1.000000000000000000),
 ( 1.000000000000000000, 0.9238795325112867385, 1.000000000000000000, 0.9238795325112867385, 1.000000000000000000, 0.9238795325112867385, 1.000000000000000000, 0.9238795325112867385, 1.000000000000000000, 0.9238795325112867385, 1.000000000000000000, 0.9238795325112867385, 1.000000000000000000, 0.9238795325112867385, 1.000000000000000000, 0.9238795325112867385, 1.000000000000000000, 0.9238795325112867385, 1.000000000000000000, 0.9238795325112867385, 1.000000000000000000, 0.9238795325112867385, 1.000000000000000000, 0.9238795325112867385, 1.000000000000000000, 0.9238795325112867385, 1.000000000000000000, 0.9238795325112867385, 1.000000000000000000, 0.9238795325112867385, 1.000000000000000000, 0.9238795325112867385, 1.000000000000000000, 0.9238795325112867385, 1.000000000000000000, 0.9238795325112867385, 1.000000000000000000, 0.9238795325112867385, 1.000000000000000000, 0.9238795325112867385, 1.000000000000000000, 0.9238795325112867385, 1.000000000000000000, 0.9238795325112867385, 1.000000000000000000, 0.9238795325112867385, 1.000000000000000000, 0.9238795325112867385, 1.000000000000000000, 0.9238795325112867385, 1.000000000000000000, 0.9238795325112867385, 1.000000000000000000, 0.9238795325112867385, 1.000000000000000000, 0.9238795325112867385, 1.000000000000000000, 0.9238795325112867385, 1.000000000000000000, 0.9238795325112867385, 1.000000000000000000, 0.9238795325112867385, 1.000000000000000000, 0.9238795325112867385, 1.000000000000000000, 0.9238795325112867385, 1.000000000000000000, 0.9238795325112867385, 1.000000000000000000, 0.9238795325112867385, 1.000000000000000000, 0.9238795325112867385, 1.000000000000000000, 0.9238795325112867385, 1.000000000000000000, 0.9238795325112867385, 1.000000000000000000, 0.9238795325112867385, 1.000000000000000000, 0.9238795325112867385, 1.000000000000000000, 0.9238795325112867385, 1.000000000000000000, 0.9238795325112867385, 1.000000000000000000, 0.9238795325112867385, 1.000000000000000000, 0.9238795325112867385, 1.000000000000000000, 0.9238795325112867385, 1.000000000000000000, 0.9238795325112867385, 1.000000000000000000, 0.9238795325112867385, 1.000000000000000000, 0.9238795325112867385, 1.000000000000000000, 0.9238795325112867385, 1.000000000000000000, 0.9238795325112867385, 1.000000000000000000, 0.9238795325112867385, 1.000000000000000000, 0.9238795325112867385, 1.000000000000000000, 0.9238795325112867385, 1.000000000000000000, 0.9238795325112867385, 1.000000000000000000, 0.9238795325112867385, 1.000000000000000000, 0.9238795325112867385, 1.000000000000000000, 0.9238795325112867385, 1.000000000000000000, 0.9238795325112867385, 1.000000000000000000, 0.9238795325112867385, 1.000000000000000000, 0.9238795325112867385, 1.000000000000000000, 0.9238795325112867385, 1.000000000000000000, 0.9238795325112867385, 1.000000000000000000, 0.9238795325112867385, 1.000000000000000000, 0.9238795325112867385, 1.000000000000000000) ) ) 
 REPRESENTATION_ITEM ( '' )  SURFACE ( )  );
#8974 = CARTESIAN_POINT ( 'NONE',  ( 20.00000000000000000, 1.500000000000003109, -17.32050807568893092 ) ) ;
#8975 = CARTESIAN_POINT ( 'NONE',  ( 4.000000000000000888, 4.898587196589412829E-16, 21.31370849898476649 ) ) ;
#8976 = EDGE_CURVE ( 'NONE', #8586, #16559, #12259, .T. ) ;
#8977 = VERTEX_POINT ( 'NONE', #15844 ) ;
#8978 = EDGE_CURVE ( 'NONE', #4760, #16067, #9253, .T. ) ;
#8979 = ORIENTED_EDGE ( 'NONE', *, *, #8635, .F. ) ;
#8980 = CARTESIAN_POINT ( 'NONE',  ( 1.656854249492381470, 4.000000000000000000, 13.81250000273119483 ) ) ;
#8981 = VERTEX_POINT ( 'NONE', #21667 ) ;
#8982 = CARTESIAN_POINT ( 'NONE',  ( 58.96875000000000711, 5.999999999999987566, 13.34314575050763452 ) ) ;
#8983 = EDGE_LOOP ( 'NONE', ( #6279, #10372, #13076, #8636 ) ) ;
#8984 = DIRECTION ( 'NONE',  ( 0.000000000000000000, -1.000000000000000000, 0.000000000000000000 ) ) ;
#8985 = ORIENTED_EDGE ( 'NONE', *, *, #10726, .T. ) ;
#8986 = CARTESIAN_POINT ( 'NONE',  ( 52.87500000000000711, 7.171572875253794166, 12.17157287525381726 ) ) ;
#8987 = CARTESIAN_POINT ( 'NONE',  ( 68.85000000218495586, 7.499999999999995559, 13.96446609406725692 ) ) ;
#8988 = DIRECTION ( 'NONE',  ( 0.3420201433256622736, 0.9396926207859106484, 0.000000000000000000 ) ) ;
#8989 = CARTESIAN_POINT ( 'NONE',  ( 2.500000000000000000, 2.629050547790028946E-15, 2.042000000000000259 ) ) ;
#8990 = DIRECTION ( 'NONE',  ( 1.000000000000000000, -0.000000000000000000, -0.000000000000000000 ) ) ;
#8991 = ORIENTED_EDGE ( 'NONE', *, *, #6606, .T. ) ;
#8992 = CARTESIAN_POINT ( 'NONE',  ( 1.656854249492381470, 4.000000000000000000, 15.81250000273119660 ) ) ;
#8993 = DIRECTION ( 'NONE',  ( 0.000000000000000000, -0.3090169943749347947, -0.9510565162951576390 ) ) ;
#8994 = CARTESIAN_POINT ( 'NONE',  ( 52.65393183416158251, 6.971812294485357775, 16.17458954617365663 ) ) ;
#8995 = LINE ( 'NONE', #18071, #3398 ) ;
#8996 = CARTESIAN_POINT ( 'NONE',  ( 66.45000000109246230, 12.06698730000000097, 14.99999999999999645 ) ) ;
#8997 = LINE ( 'NONE', #5026, #16133 ) ;
#8998 = EDGE_LOOP ( 'NONE', ( #17680, #13478 ) ) ;
#8999 = CARTESIAN_POINT ( 'NONE',  ( -1.515948947685982429, 3.114950916665994995, -3.295601554149324208 ) ) ;
#9000 = CARTESIAN_POINT ( 'NONE',  ( 54.56250000000000711, 6.999999999999997335, 15.00000000000000533 ) ) ;
#9001 = DIRECTION ( 'NONE',  ( 1.000000000000000000, 0.000000000000000000, 0.000000000000000000 ) ) ;
#9002 = CARTESIAN_POINT ( 'NONE',  ( -72.50000000000000000, 9.999999999999998224, 17.49999999999999645 ) ) ;
#9003 = ADVANCED_FACE ( 'NONE', ( #1556 ), #18350, .T. ) ;
#9004 = EDGE_CURVE ( 'NONE', #2984, #10612, #23300, .T. ) ;
#9005 = ORIENTED_EDGE ( 'NONE', *, *, #12635, .F. ) ;
#9006 = LINE ( 'NONE', #19978, #7854 ) ;
#9007 = CARTESIAN_POINT ( 'NONE',  ( 3.458734125000000770, -1.432654583217639610, -1.824999998634404097 ) ) ;
#9008 = DIRECTION ( 'NONE',  ( 1.000000000000000000, 7.703719777548943412E-32, 0.000000000000000000 ) ) ;
#9009 = ORIENTED_EDGE ( 'NONE', *, *, #6933, .F. ) ;
#9010 = CARTESIAN_POINT ( 'NONE',  ( 70.04999999999999716, 11.03553390593273420, 17.50000000000000711 ) ) ;
#9011 = ORIENTED_EDGE ( 'NONE', *, *, #3034, .T. ) ;
#9012 = CARTESIAN_POINT ( 'NONE',  ( -1.656854249492379250, 4.000000000000000000, 16.81250000000001066 ) ) ;
#9013 = LINE ( 'NONE', #3700, #5756 ) ;
#9014 = APPLICATION_CONTEXT ( 'automotive_design' ) ;
#9015 = LINE ( 'NONE', #17978, #3786 ) ;
#9016 = DIRECTION ( 'NONE',  ( 0.9413949561959079615, 0.3373062947069096484, -0.000000000000000000 ) ) ;
#9017 = CARTESIAN_POINT ( 'NONE',  ( 0.000000000000000000, 0.000000000000000000, 3.059999999999998277 ) ) ;
#9018 = VECTOR ( 'NONE', #571, 1000.000000000000000 ) ;
#9019 = CARTESIAN_POINT ( 'NONE',  ( -67.29999999999999716, 9.999999999999998224, 12.49999999999999289 ) ) ;
#9020 = VECTOR ( 'NONE', #19946, 1000.000000000000000 ) ;
#9021 = CARTESIAN_POINT ( 'NONE',  ( -19.99999999999999645, -9.000000000000003553, 10.00000000000008882 ) ) ;
#9022 = CARTESIAN_POINT ( 'NONE',  ( 3.458734125000001214, 4.235727675282971730E-16, 17.93750000136560274 ) ) ;
#9023 = PLANE ( 'NONE',  #3616 ) ;
#9024 = CARTESIAN_POINT ( 'NONE',  ( -1.656854249492380804, 4.000000000000000000, 4.112500000000001599 ) ) ;
#9025 = CARTESIAN_POINT ( 'NONE',  ( -4.000000000000000000, 0.000000000000000000, 0.3000000000000016542 ) ) ;
#9026 = CARTESIAN_POINT ( 'NONE',  ( 67.95000000000001705, 7.499999999999996447, 13.96446609406725514 ) ) ;
#9027 = CARTESIAN_POINT ( 'NONE',  ( 1.432654583217641164, 3.458734125000000326, 16.12500000136560629 ) ) ;
#9028 = LINE ( 'NONE', #21556, #3067 ) ;
#9029 = VERTEX_POINT ( 'NONE', #10698 ) ;
#9030 = CARTESIAN_POINT ( 'NONE',  ( -69.45000000109247651, 12.06698730000000097, 14.99999999999999645 ) ) ;
#9031 = EDGE_LOOP ( 'NONE', ( #73, #10521, #6366, #7957 ) ) ;
#9032 = CARTESIAN_POINT ( 'NONE',  ( 52.84143183416158251, 8.275094609562001935, 18.97181229448536044 ) ) ;
#9033 = CARTESIAN_POINT ( 'NONE',  ( -65.95000000109247651, 8.538419263543524096, 13.53841926354352054 ) ) ;
#9034 = CARTESIAN_POINT ( 'NONE',  ( -2.445694354108820523, 2.445694354108820523, -1.387499998634402987 ) ) ;
#9035 = ORIENTED_EDGE ( 'NONE', *, *, #91, .F. ) ;
#9036 = AXIS2_PLACEMENT_3D ( 'NONE', #22523, #6492, #11903 ) ;
#9037 = ORIENTED_EDGE ( 'NONE', *, *, #1471, .T. ) ;
#9038 = CIRCLE ( 'NONE', #6354, 5.000000000000000888 ) ;
#9039 = CARTESIAN_POINT ( 'NONE',  ( 58.78125000000000711, 8.757359312880703683, 11.99999999999999822 ) ) ;
#9040 = EDGE_CURVE ( 'NONE', #13240, #22158, #23476, .T. ) ;
#9041 = CARTESIAN_POINT ( 'NONE',  ( -69.75000000109247367, 8.538419263543522320, 16.46158073645647235 ) ) ;
#9042 = CIRCLE ( 'NONE', #16046, 5.000000000000000888 ) ;
#9043 = AXIS2_PLACEMENT_3D ( 'NONE', #8375, #21144, #11626 ) ;
#9044 = CARTESIAN_POINT ( 'NONE',  ( -70.65000000109246514, 9.999999999999998224, 17.06698730000000097 ) ) ;
#9045 = CARTESIAN_POINT ( 'NONE',  ( -3.458734124999999437, 1.432654583217640498, 13.62500000136560452 ) ) ;
#9046 = DIRECTION ( 'NONE',  ( -1.000000000000000000, -0.000000000000000000, 0.000000000000000000 ) ) ;
#9047 = CARTESIAN_POINT ( 'NONE',  ( 52.68750000000000711, 9.999999999999989342, 11.99999999999999467 ) ) ;
#9048 = FACE_OUTER_BOUND ( 'NONE', #23166, .T. ) ;
#9049 = CARTESIAN_POINT ( 'NONE',  ( 55.03125000000000000, 11.24264068711929276, 18.00000000000000355 ) ) ;
#9050 = CARTESIAN_POINT ( 'NONE',  ( -2.272871948086449656, -2.616781258933798426, 2.039999999999998259 ) ) ;
#9051 = FACE_OUTER_BOUND ( 'NONE', #11548, .T. ) ;
#9052 = ORIENTED_EDGE ( 'NONE', *, *, #4155, .T. ) ;
#9053 = CARTESIAN_POINT ( 'NONE',  ( -0.3649867057748841237, 3.983313282257322285, 21.31370849898476649 ) ) ;
#9054 = DIRECTION ( 'NONE',  ( 0.000000000000000000, 0.000000000000000000, -1.000000000000000000 ) ) ;
#9055 = ORIENTED_EDGE ( 'NONE', *, *, #2676, .F. ) ;
#9056 = CARTESIAN_POINT ( 'NONE',  ( 56.06250000000000000, 6.999999999999997335, 15.00000000000000533 ) ) ;
#9057 =( LENGTH_UNIT ( ) NAMED_UNIT ( * ) SI_UNIT ( .MILLI., .METRE. ) );
#9058 = CARTESIAN_POINT ( 'NONE',  ( -4.000000000000000000, -1.656854249492383246, -3.512499997268812901 ) ) ;
#9059 = FACE_OUTER_BOUND ( 'NONE', #11924, .T. ) ;
#9060 = ORIENTED_EDGE ( 'NONE', *, *, #3938, .T. ) ;
#9061 = CARTESIAN_POINT ( 'NONE',  ( -2.828427124746188515, -2.828427124746190735, 18.12500000000001066 ) ) ;
#9062 = ORIENTED_EDGE ( 'NONE', *, *, #23074, .T. ) ;
#9063 = DIRECTION ( 'NONE',  ( 0.000000000000000000, 0.000000000000000000, -1.000000000000000000 ) ) ;
#9064 = CARTESIAN_POINT ( 'NONE',  ( -2.247776618166720475, 3.308700692843488333, 9.970592379354943802 ) ) ;
#9065 = ORIENTED_EDGE ( 'NONE', *, *, #5667, .F. ) ;
#9066 = CARTESIAN_POINT ( 'NONE',  ( -17.30284271966725029, -11.25000000000000355, 10.00000000000008882 ) ) ;
#9067 = EDGE_CURVE ( 'NONE', #9624, #428, #9015, .T. ) ;
#9068 = FACE_OUTER_BOUND ( 'NONE', #18346, .T. ) ;
#9069 = ADVANCED_FACE ( 'NONE', ( #18440, #1787 ), #10928, .T. ) ;
#9070 = CARTESIAN_POINT ( 'NONE',  ( 4.000000000000000000, 2.309401076758515803, -0.4999999999999995559 ) ) ;
#9071 = EDGE_CURVE ( 'NONE', #2045, #12358, #17593, .T. ) ;
#9072 = CARTESIAN_POINT ( 'NONE',  ( 70.29999999999999716, 7.499999999999996447, 14.99999999999999645 ) ) ;
#9073 = ADVANCED_FACE ( 'NONE', ( #21791 ), #18326, .F. ) ;
#9074 = FACE_OUTER_BOUND ( 'NONE', #19422, .T. ) ;
#9075 = CARTESIAN_POINT ( 'NONE',  ( 27.50000000000000000, 4.500000000000006217, -31.01025403784446510 ) ) ;
#9076 = CARTESIAN_POINT ( 'NONE',  ( 53.65856816583844591, 6.028187705514649330, 16.72490539043803182 ) ) ;
#9077 = CARTESIAN_POINT ( 'NONE',  ( 3.458734125000000770, -1.432654583217639610, 1.175000001365597013 ) ) ;
#9078 = LINE ( 'NONE', #10879, #17946 ) ;
#9079 = FACE_OUTER_BOUND ( 'NONE', #22218, .T. ) ;
#9080 = VECTOR ( 'NONE', #1674, 1000.000000000000000 ) ;
#9081 = CARTESIAN_POINT ( 'NONE',  ( -10.00000000000000000, 0.000000000000000000, 0.000000000000000000 ) ) ;
#9082 = ORIENTED_EDGE ( 'NONE', *, *, #15696, .F. ) ;
#9083 = FACE_OUTER_BOUND ( 'NONE', #17969, .T. ) ;
#9084 = CARTESIAN_POINT ( 'NONE',  ( 44.10446624071656174, -8.974600000000002353, 5.000000000000079936 ) ) ;
#9085 = DIRECTION ( 'NONE',  ( -1.000000000000000000, -7.703719777548943412E-32, 0.000000000000000000 ) ) ;
#9086 = EDGE_LOOP ( 'NONE', ( #20204, #19567, #8361, #19972 ) ) ;
#9087 = ORIENTED_EDGE ( 'NONE', *, *, #23158, .F. ) ;
#9088 = DIRECTION ( 'NONE',  ( -1.000000000000000000, 0.000000000000000000, 0.000000000000000000 ) ) ;
#9089 = CARTESIAN_POINT ( 'NONE',  ( 55.78125000000000711, 8.343145750507600766, 11.00000000000000355 ) ) ;
#9090 = VERTEX_POINT ( 'NONE', #18209 ) ;
#9091 = CARTESIAN_POINT ( 'NONE',  ( 4.000000000000001776, -1.656854249492379694, 18.43750000000001066 ) ) ;
#9092 = ORIENTED_EDGE ( 'NONE', *, *, #6897, .T. ) ;
#9093 = VECTOR ( 'NONE', #2077, 1000.000000000000000 ) ;
#9094 = CARTESIAN_POINT ( 'NONE',  ( 57.40856816583844591, 13.97181229448534978, 13.27509460956196641 ) ) ;
#9095 = EDGE_CURVE ( 'NONE', #21366, #17500, #7085, .T. ) ;
#9096 = CARTESIAN_POINT ( 'NONE',  ( 69.55000000218495870, 7.499999999999995559, 16.03553390593273420 ) ) ;
#9097 = CARTESIAN_POINT ( 'NONE',  ( -10.01919788420863711, -5.367285115750873636, 10.00000000000008882 ) ) ;
#9098 = DIRECTION ( 'NONE',  ( -1.000000000000000000, -0.000000000000000000, 0.000000000000000000 ) ) ;
#9099 = DIRECTION ( 'NONE',  ( 0.000000000000000000, 0.000000000000000000, 1.000000000000000000 ) ) ;
#9100 = EDGE_CURVE ( 'NONE', #20911, #14597, #5869, .T. ) ;
#9101 = ORIENTED_EDGE ( 'NONE', *, *, #8530, .F. ) ;
#9102 = CARTESIAN_POINT ( 'NONE',  ( -2.828427124746189403, 2.828427124746190291, 17.00000000273119838 ) ) ;
#9103 = EDGE_CURVE ( 'NONE', #9988, #6003, #3036, .T. ) ;
#9104 = VECTOR ( 'NONE', #19581, 1000.000000000000000 ) ;
#9105 = DIRECTION ( 'NONE',  ( 0.000000000000000000, 0.000000000000000000, 1.000000000000000000 ) ) ;
#9106 =( BOUNDED_SURFACE ( )  B_SPLINE_SURFACE ( 3, 2, ( 
 ( #20203, #208, #5610 ),
 ( #16630, #1999, #457 ),
 ( #13292, #7539, #11024 ),
 ( #1771, #11147, #21883 ),
 ( #18421, #19844, #14858 ),
 ( #5491, #7428, #1890 ) ),
 .UNSPECIFIED., .F., .F., .F. ) 
 B_SPLINE_SURFACE_WITH_KNOTS ( ( 4, 2, 4 ),
 ( 3, 3 ),
 ( 0.02027065861071770947, 0.02273072267836921331, 0.02519078674602071716 ),
 ( 0.000000000000000000, 1.000000000000000000 ),
 .UNSPECIFIED. ) 
 GEOMETRIC_REPRESENTATION_ITEM ( )  RATIONAL_B_SPLINE_SURFACE ( (
 ( 1.000000000000000000, 0.8047781708337304885, 1.000000000000000000),
 ( 1.000000000000000000, 0.8123765190705307671, 1.000000000000000000),
 ( 1.000000000000000000, 0.8190656277163975707, 1.000000000000000000),
 ( 1.000000000000000000, 0.8192366903512159348, 1.000000000000000000),
 ( 1.000000000000000000, 0.8126138454302893610, 1.000000000000000000),
 ( 1.000000000000000000, 0.8047712246031417660, 1.000000000000000000) ) ) 
 REPRESENTATION_ITEM ( '' )  SURFACE ( )  );
#9107 = CARTESIAN_POINT ( 'NONE',  ( 56.96643183416158251, 6.028187705514633343, 13.27509460956200016 ) ) ;
#9108 = DIRECTION ( 'NONE',  ( -7.087422195345011518E-32, -1.000000000000000000, -0.000000000000000000 ) ) ;
#9109 = CARTESIAN_POINT ( 'NONE',  ( 67.00000000218494733, 9.999999999999998224, 17.49999999999999645 ) ) ;
#9110 = AXIS2_PLACEMENT_3D ( 'NONE', #15434, #21010, #15554 ) ;
#9111 = CARTESIAN_POINT ( 'NONE',  ( -68.09999999999999432, 9.999999999999998224, 12.49999999999999289 ) ) ;
#9112 = TOROIDAL_SURFACE ( 'NONE', #5651, 8.239200000000002078, 0.03079999999999868954 ) ;
#9113 = DIRECTION ( 'NONE',  ( -1.000000000000000000, -0.000000000000000000, -0.000000000000000000 ) ) ;
#9114 = EDGE_LOOP ( 'NONE', ( #16850, #13570, #10044, #3663 ) ) ;
#9115 = CARTESIAN_POINT ( 'NONE',  ( 1.506022603841227436, 0.000000000000000000, -8.265000000000021885 ) ) ;
#9116 = CARTESIAN_POINT ( 'NONE',  ( 58.59375000000000711, 11.24264068711927322, 11.99999999999998934 ) ) ;
#9117 = DIRECTION ( 'NONE',  ( 0.3420201433256622181, 0.9396926207859107594, -6.162975822039141593E-32 ) ) ;
#9118 = SURFACE_STYLE_FILL_AREA ( #16523 ) ;
#9119 = ORIENTED_EDGE ( 'NONE', *, *, #16704, .F. ) ;
#9120 = LINE ( 'NONE', #14514, #10564 ) ;
#9121 = VECTOR ( 'NONE', #2305, 1000.000000000000000 ) ;
#9122 = DIRECTION ( 'NONE',  ( 0.000000000000000000, -1.000000000000000000, 0.000000000000000000 ) ) ;
#9123 = CARTESIAN_POINT ( 'NONE',  ( 2.000000000000001776, 0.000000000000000000, 0.000000000000000000 ) ) ;
#9124 = ORIENTED_EDGE ( 'NONE', *, *, #22569, .F. ) ;
#9125 = DIRECTION ( 'NONE',  ( -1.000000000000000000, 0.000000000000000000, 0.000000000000000000 ) ) ;
#9126 = ORIENTED_EDGE ( 'NONE', *, *, #12196, .F. ) ;
#9127 = CIRCLE ( 'NONE', #1437, 11.00000000000000000 ) ;
#9128 = CARTESIAN_POINT ( 'NONE',  ( 72.50000000000000000, 9.999999999999998224, 12.49999999999999289 ) ) ;
#9129 = CARTESIAN_POINT ( 'NONE',  ( -1.432654583217639166, 3.458734125000000770, 10.50000000136560629 ) ) ;
#9130 = LINE ( 'NONE', #5395, #22593 ) ;
#9131 = AXIS2_PLACEMENT_3D ( 'NONE', #7267, #16356, #3755 ) ;
#9132 = VECTOR ( 'NONE', #1218, 1000.000000000000000 ) ;
#9133 = CARTESIAN_POINT ( 'NONE',  ( 4.999999999999999112, 0.000000000000000000, 0.000000000000000000 ) ) ;
#9134 = EDGE_CURVE ( 'NONE', #6815, #4263, #1673, .T. ) ;
#9135 = CARTESIAN_POINT ( 'NONE',  ( 22.10407284676620066, -9.000000000000001776, 5.000000000000079936 ) ) ;
#9136 = ADVANCED_FACE ( 'NONE', ( #16649 ), #1911, .F. ) ;
#9137 = DIRECTION ( 'NONE',  ( 0.000000000000000000, 0.000000000000000000, -1.000000000000000000 ) ) ;
#9138 = EDGE_CURVE ( 'NONE', #13563, #6932, #9252, .T. ) ;
#9139 = CIRCLE ( 'NONE', #12199, 2.500000000000002220 ) ;
#9140 = CARTESIAN_POINT ( 'NONE',  ( -66.29999999999999716, 7.499999999999996447, 14.99999999999999645 ) ) ;
#9141 = DIRECTION ( 'NONE',  ( 0.000000000000000000, 1.000000000000000000, -1.224646799147353207E-16 ) ) ;
#9142 = CARTESIAN_POINT ( 'NONE',  ( 1.432654583217641164, 3.458734125000000326, 18.12500000136560274 ) ) ;
#9143 = DIRECTION ( 'NONE',  ( -0.000000000000000000, -1.000000000000000000, 0.000000000000000000 ) ) ;
#9144 = AXIS2_PLACEMENT_3D ( 'NONE', #3124, #15619, #10588 ) ;
#9145 = CARTESIAN_POINT ( 'NONE',  ( 2.445694354108820079, 2.445694354108820523, -2.387499998634403653 ) ) ;
#9146 = DIRECTION ( 'NONE',  ( 0.000000000000000000, 0.000000000000000000, 1.000000000000000000 ) ) ;
#9147 = CARTESIAN_POINT ( 'NONE',  ( 3.458734125000002102, -1.432654583217639610, 14.87500000136560807 ) ) ;
#9148 = DIRECTION ( 'NONE',  ( 0.000000000000000000, 0.000000000000000000, 1.000000000000000000 ) ) ;
#9149 = ORIENTED_EDGE ( 'NONE', *, *, #11134, .T. ) ;
#9150 = CIRCLE ( 'NONE', #17111, 6.500000000000000888 ) ;
#9151 = CARTESIAN_POINT ( 'NONE',  ( -69.20000000109246230, 9.143825827087052716, 12.93301269999999192 ) ) ;
#9152 = ORIENTED_EDGE ( 'NONE', *, *, #13877, .T. ) ;
#9153 = CARTESIAN_POINT ( 'NONE',  ( 57.62268183416157541, 12.78030770151606177, 17.87654654797631792 ) ) ;
#9154 = CARTESIAN_POINT ( 'NONE',  ( -66.15000000109247935, 11.46158073645647235, 13.53841926354352232 ) ) ;
#9155 = CARTESIAN_POINT ( 'NONE',  ( 0.000000000000000000, 0.000000000000000000, 29.99999999999998934 ) ) ;
#9156 = AXIS2_PLACEMENT_3D ( 'NONE', #15513, #22782, #6390 ) ;
#9157 = CARTESIAN_POINT ( 'NONE',  ( -1.656854249492380138, -3.999999999999999112, 17.18750000000001066 ) ) ;
#9158 = ORIENTED_EDGE ( 'NONE', *, *, #13888, .T. ) ;
#9159 = EDGE_LOOP ( 'NONE', ( #7649, #23592, #5829, #8177 ) ) ;
#9160 = DIRECTION ( 'NONE',  ( 0.000000000000000000, 0.000000000000000000, -1.000000000000000000 ) ) ;
#9161 = VECTOR ( 'NONE', #5280, 1000.000000000000000 ) ;
#9162 = CARTESIAN_POINT ( 'NONE',  ( 52.81481816583844591, 12.99999999999999822, 14.93194885905435676 ) ) ;
#9163 = VECTOR ( 'NONE', #11406, 1000.000000000000000 ) ;
#9164 = CARTESIAN_POINT ( 'NONE',  ( -69.35000000109248219, 11.46158073645647235, 13.53841926354352232 ) ) ;
#9165 = ADVANCED_FACE ( 'NONE', ( #6967 ), #11043, .T. ) ;
#9166 = CARTESIAN_POINT ( 'NONE',  ( -70.70000000109247651, 9.143825827087049163, 17.06698729999999742 ) ) ;
#9167 = VECTOR ( 'NONE', #20332, 1000.000000000000000 ) ;
#9168 = CARTESIAN_POINT ( 'NONE',  ( 1.432654583217643163, -3.458734124999999882, 13.00000000136560629 ) ) ;
#9169 = DIRECTION ( 'NONE',  ( 1.000000000000000000, 7.703719777548943412E-32, 0.000000000000000000 ) ) ;
#9170 = CARTESIAN_POINT ( 'NONE',  ( 53.43750000000000711, 10.00000000000000711, 17.99999999999999645 ) ) ;
#9171 = DIRECTION ( 'NONE',  ( 0.000000000000000000, 0.000000000000000000, -1.000000000000000000 ) ) ;
#9172 = AXIS2_PLACEMENT_3D ( 'NONE', #18072, #21276, #1180 ) ;
#9173 = CARTESIAN_POINT ( 'NONE',  ( 53.25000000000000711, 7.878679656440361612, 17.12132034355964549 ) ) ;
#9174 = CARTESIAN_POINT ( 'NONE',  ( 0.2373759324227673606, -3.458017446235651438, 2.039999999999998259 ) ) ;
#9175 = VECTOR ( 'NONE', #20104, 1000.000000000000000 ) ;
#9176 = FACE_OUTER_BOUND ( 'NONE', #19687, .T. ) ;
#9177 = VECTOR ( 'NONE', #12820, 1000.000000000000000 ) ;
#9178 = ORIENTED_EDGE ( 'NONE', *, *, #12356, .F. ) ;
#9179 = CYLINDRICAL_SURFACE ( 'NONE', #7177, 4.000000000000000000 ) ;
#9180 = LINE ( 'NONE', #12774, #1314 ) ;
#9181 = ORIENTED_EDGE ( 'NONE', *, *, #5865, .T. ) ;
#9182 = CARTESIAN_POINT ( 'NONE',  ( 51.84375000000001421, 8.757359312880723223, 18.00000000000000355 ) ) ;
#9183 = CARTESIAN_POINT ( 'NONE',  ( -2.117863837641485618E-16, 3.458734125000000326, 4.487500001365595459 ) ) ;
#9184 = CARTESIAN_POINT ( 'NONE',  ( -2.500000000000000444, 3.061616997868383634E-16, -25.03750572909317285 ) ) ;
#9185 = ORIENTED_EDGE ( 'NONE', *, *, #1837, .F. ) ;
#9186 = EDGE_CURVE ( 'NONE', #15974, #18318, #7197, .T. ) ;
#9187 = CARTESIAN_POINT ( 'NONE',  ( -3.999999999999999112, 1.656854249492380804, 15.93750000000001066 ) ) ;
#9188 = CARTESIAN_POINT ( 'NONE',  ( -1.600000000000004086, 8.247996192257451316E-16, 6.735000000000022524 ) ) ;
#9189 = AXIS2_PLACEMENT_3D ( 'NONE', #21601, #23532, #12786 ) ;
#9190 = DIRECTION ( 'NONE',  ( -1.000000000000000000, -0.000000000000000000, -0.000000000000000000 ) ) ;
#9191 = ORIENTED_EDGE ( 'NONE', *, *, #18062, .F. ) ;
#9192 = DIRECTION ( 'NONE',  ( -0.000000000000000000, -1.000000000000000000, -0.000000000000000000 ) ) ;
#9193 = VECTOR ( 'NONE', #12926, 1000.000000000000114 ) ;
#9194 = CARTESIAN_POINT ( 'NONE',  ( -2.117863837641485618E-16, 3.458734125000000770, -0.2624999986344037084 ) ) ;
#9195 = CIRCLE ( 'NONE', #17595, 4.000000000000001776 ) ;
#9196 = CARTESIAN_POINT ( 'NONE',  ( 68.74999999999998579, 7.499999999999995559, 13.96446609406725692 ) ) ;
#9197 = DIRECTION ( 'NONE',  ( -1.000000000000000000, 0.000000000000000000, -0.000000000000000000 ) ) ;
#9198 = DIRECTION ( 'NONE',  ( 1.000000000000000000, -0.000000000000000000, -0.000000000000000000 ) ) ;
#9199 = VECTOR ( 'NONE', #1007, 1000.000000000000000 ) ;
#9200 = CARTESIAN_POINT ( 'NONE',  ( 51.03356816583844591, 11.72490539043803004, 18.97181229448534268 ) ) ;
#9201 = CARTESIAN_POINT ( 'NONE',  ( 2.445694354108820523, -2.445694354108820079, -1.887499998634403431 ) ) ;
#9202 = CARTESIAN_POINT ( 'NONE',  ( 45.00000000000000000, 2.399706452296377801, 55.00000000000021316 ) ) ;
#9203 = CARTESIAN_POINT ( 'NONE',  ( 4.000000000000001776, -1.656854249492379694, 18.56250000273119838 ) ) ;
#9204 = ADVANCED_FACE ( 'NONE', ( #11169, #9359 ), #14284, .F. ) ;
#9205 = CARTESIAN_POINT ( 'NONE',  ( -2.828427124746189403, 2.828427124746190291, 16.87500000000001066 ) ) ;
#9206 = ORIENTED_EDGE ( 'NONE', *, *, #11731, .T. ) ;
#9207 = DIRECTION ( 'NONE',  ( -4.625929269271486900E-16, 1.000000000000000000, 5.665129472695380173E-32 ) ) ;
#9208 = CARTESIAN_POINT ( 'NONE',  ( -65.00000000000000000, -10.00000000000000178, 14.99999999999999467 ) ) ;
#9209 = LINE ( 'NONE', #21742, #18918 ) ;
#9210 = EDGE_LOOP ( 'NONE', ( #5181, #8642, #21349, #2121 ) ) ;
#9211 = AXIS2_PLACEMENT_3D ( 'NONE', #12405, #19670, #10618 ) ;
#9212 = VERTEX_POINT ( 'NONE', #2138 ) ;
#9213 = ORIENTED_EDGE ( 'NONE', *, *, #12262, .F. ) ;
#9214 = ADVANCED_FACE ( 'NONE', ( #13194 ), #14879, .T. ) ;
#9215 = CARTESIAN_POINT ( 'NONE',  ( 56.25000000000000711, 7.171572875253819923, 17.82842712474619873 ) ) ;
#9216 = ORIENTED_EDGE ( 'NONE', *, *, #2676, .T. ) ;
#9217 = FACE_OUTER_BOUND ( 'NONE', #21169, .T. ) ;
#9218 = ORIENTED_EDGE ( 'NONE', *, *, #15566, .T. ) ;
#9219 = VECTOR ( 'NONE', #18051, 1000.000000000000114 ) ;
#9220 = CARTESIAN_POINT ( 'NONE',  ( 55.90856816583843880, 13.97181229448534978, 13.27509460956196641 ) ) ;
#9221 = AXIS2_PLACEMENT_3D ( 'NONE', #154, #16574, #9401 ) ;
#9222 = CARTESIAN_POINT ( 'NONE',  ( 71.55000000109247082, 8.538419263543524096, 13.53841926354352054 ) ) ;
#9223 = CARTESIAN_POINT ( 'NONE',  ( -3.999999999999998224, -1.656854249492383024, 16.06250000000001066 ) ) ;
#9224 = CARTESIAN_POINT ( 'NONE',  ( 0.000000000000000000, 0.000000000000000000, 2.040000000000001812 ) ) ;
#9225 = VERTEX_POINT ( 'NONE', #22255 ) ;
#9226 = CARTESIAN_POINT ( 'NONE',  ( -3.999999999999999112, -2.265485919601331943, 19.21045885948849019 ) ) ;
#9227 = CARTESIAN_POINT ( 'NONE',  ( -3.511755186886750479, 2.826662030176366081, -3.597382984111578086 ) ) ;
#9228 = CARTESIAN_POINT ( 'NONE',  ( 56.31018183416157541, 14.00000000000000000, 15.06805114094561304 ) ) ;
#9229 = DIRECTION ( 'NONE',  ( 0.000000000000000000, 0.000000000000000000, -1.000000000000000000 ) ) ;
#9230 = LINE ( 'NONE', #9451, #7069 ) ;
#9231 = LINE ( 'NONE', #16517, #12835 ) ;
#9232 = EDGE_CURVE ( 'NONE', #21915, #18272, #23696, .T. ) ;
#9233 = LINE ( 'NONE', #16401, #10369 ) ;
#9234 = VERTEX_POINT ( 'NONE', #7557 ) ;
#9235 = CARTESIAN_POINT ( 'NONE',  ( 0.000000000000000000, 0.000000000000000000, -3.700000000000000178 ) ) ;
#9236 = EDGE_CURVE ( 'NONE', #22617, #21471, #1498, .T. ) ;
#9237 = CARTESIAN_POINT ( 'NONE',  ( 51.28125000000000000, 8.757359312880703683, 11.99999999999999822 ) ) ;
#9238 = CYLINDRICAL_SURFACE ( 'NONE', #17358, 4.000000000000001776 ) ;
#9239 = ORIENTED_EDGE ( 'NONE', *, *, #20791, .T. ) ;
#9240 = CARTESIAN_POINT ( 'NONE',  ( -4.000000000000000000, 0.000000000000000000, -3.574999997268813345 ) ) ;
#9241 = CARTESIAN_POINT ( 'NONE',  ( -3.458734124999999882, -1.432654583217642497, -0.1999999986344043745 ) ) ;
#9242 = LINE ( 'NONE', #22125, #15550 ) ;
#9243 = EDGE_CURVE ( 'NONE', #3610, #10634, #21909, .T. ) ;
#9244 = ORIENTED_EDGE ( 'NONE', *, *, #22966, .T. ) ;
#9245 = CARTESIAN_POINT ( 'NONE',  ( 4.000000000000000888, 1.539600717838996990, -3.300726591567079815 ) ) ;
#9246 = EDGE_LOOP ( 'NONE', ( #20597, #7800, #13125, #15727 ) ) ;
#9247 = ADVANCED_FACE ( 'NONE', ( #15354 ), #13082, .F. ) ;
#9248 = CARTESIAN_POINT ( 'NONE',  ( -20.00005079999999680, 0.000000000000000000, 4.000000000000000000 ) ) ;
#9249 = CARTESIAN_POINT ( 'NONE',  ( 1.656854249492381470, 4.000000000000000000, 17.68750000000001066 ) ) ;
#9250 = DIRECTION ( 'NONE',  ( 0.000000000000000000, 0.000000000000000000, -1.000000000000000000 ) ) ;
#9251 = VECTOR ( 'NONE', #561, 1000.000000000000000 ) ;
#9252 = LINE ( 'NONE', #20222, #750 ) ;
#9253 =( BOUNDED_CURVE ( )  B_SPLINE_CURVE ( 2, ( #19638, #3238, #21185, #4802, #4922, #19526, #3123, #3590, #5398 ),
 .UNSPECIFIED., .F., .F. ) 
 B_SPLINE_CURVE_WITH_KNOTS ( ( 3, 2, 2, 2, 3 ),
 ( 0.5625000000000008882, 0.5781250000000007772, 0.5937500000000006661, 0.6093750000000006661, 0.6250000000000005551 ),
 .UNSPECIFIED. ) 
 CURVE ( )  GEOMETRIC_REPRESENTATION_ITEM ( )  RATIONAL_B_SPLINE_CURVE ( ( 0.9999999999999956701, 0.9238795325112910684, 1.000000000000000000, 0.9238795325112867385, 1.000000000000000000, 0.9238795325112867385, 1.000000000000000000, 0.9238795325112840739, 1.000000000000002665 ) ) 
 REPRESENTATION_ITEM ( '' )  );
#9254 = DIRECTION ( 'NONE',  ( -0.3373062947069096484, 0.9413949561959079615, 0.000000000000000000 ) ) ;
#9255 = ORIENTED_EDGE ( 'NONE', *, *, #17706, .F. ) ;
#9256 = CARTESIAN_POINT ( 'NONE',  ( -67.99999999999998579, 8.232233047033629347, 13.23223304703362402 ) ) ;
#9257 = LINE ( 'NONE', #18213, #2249 ) ;
#9258 = CARTESIAN_POINT ( 'NONE',  ( 72.20000000109246230, 10.85617417291294551, 17.06698729999999742 ) ) ;
#9259 = CARTESIAN_POINT ( 'NONE',  ( -3.458734124999998993, -1.432654583217642497, 16.50000000136560629 ) ) ;
#9260 = PLANE ( 'NONE',  #10361 ) ;
#9261 = CARTESIAN_POINT ( 'NONE',  ( 1.656854249492380360, 4.000000000000000000, 5.987500000000000711 ) ) ;
#9262 = EDGE_CURVE ( 'NONE', #4473, #2044, #11757, .T. ) ;
#9263 = CARTESIAN_POINT ( 'NONE',  ( 44.70083240928345703, -8.974600000000002353, 5.000000000000079936 ) ) ;
#9264 = CARTESIAN_POINT ( 'NONE',  ( -3.458734124999998993, 0.000000000000000000, 12.43750000136560629 ) ) ;
#9265 = CARTESIAN_POINT ( 'NONE',  ( 4.999999999999999112, 9.241976615262133876, 1.699438267350532827 ) ) ;
#9266 = ORIENTED_EDGE ( 'NONE', *, *, #8838, .T. ) ;
#9267 = CARTESIAN_POINT ( 'NONE',  ( -67.65000000109247935, 9.999999999999998224, 12.93301269999999192 ) ) ;
#9268 = ORIENTED_EDGE ( 'NONE', *, *, #10738, .F. ) ;
#9269 = CARTESIAN_POINT ( 'NONE',  ( 56.02893183416158962, 11.58880310854676132, 19.02818770551463956 ) ) ;
#9270 = CARTESIAN_POINT ( 'NONE',  ( -70.40000000109247935, 12.06698730000000275, 14.14382582708705094 ) ) ;
#9271 = APPLICATION_PROTOCOL_DEFINITION ( 'draft international standard', 'automotive_design', 1998, #3495 ) ;
#9272 = DIRECTION ( 'NONE',  ( 1.000000000000000000, 0.000000000000000000, -0.000000000000000000 ) ) ;
#9273 = ORIENTED_EDGE ( 'NONE', *, *, #23233, .F. ) ;
#9274 = ADVANCED_FACE ( 'NONE', ( #22495 ), #3422, .T. ) ;
#9275 = ORIENTED_EDGE ( 'NONE', *, *, #5455, .T. ) ;
#9276 = CARTESIAN_POINT ( 'NONE',  ( 2.445694354108821411, 2.445694354108820523, 19.31250000136560629 ) ) ;
#9277 = CARTESIAN_POINT ( 'NONE',  ( 52.15856816583843880, 7.028187705514647554, 16.31069182806492179 ) ) ;
#9278 = CARTESIAN_POINT ( 'NONE',  ( -70.55000000109247082, 8.538419263543522320, 16.46158073645647235 ) ) ;
#9279 = CARTESIAN_POINT ( 'NONE',  ( -71.50000000109247367, 9.143825827087049163, 17.06698729999999742 ) ) ;
#9280 = CARTESIAN_POINT ( 'NONE',  ( 3.458734125000001658, 1.432654583217640498, 12.25000000136560629 ) ) ;
#9281 = CARTESIAN_POINT ( 'NONE',  ( -4.211140560182196957, -2.431303136016552013, -3.745885042887436178 ) ) ;
#9282 = CARTESIAN_POINT ( 'NONE',  ( 60.71643183416158962, 12.97181229448535689, 16.31069182806490758 ) ) ;
#9283 = CARTESIAN_POINT ( 'NONE',  ( 0.000000000000000000, 0.000000000000000000, -4.484454397937119197 ) ) ;
#9284 = CARTESIAN_POINT ( 'NONE',  ( 54.18750000000000711, 9.999999999999989342, 11.99999999999999467 ) ) ;
#9285 = CARTESIAN_POINT ( 'NONE',  ( 9.920644283265380691E-16, 4.000000000000000000, 17.87500000273119483 ) ) ;
#9286 = CARTESIAN_POINT ( 'NONE',  ( -19.99999999999999645, -9.000000000000003553, 5.000000000000079936 ) ) ;
#9287 = ORIENTED_EDGE ( 'NONE', *, *, #17805, .F. ) ;
#9288 = CARTESIAN_POINT ( 'NONE',  ( -90.00000000000000000, 0.000000000000000000, 0.000000000000000000 ) ) ;
#9289 = CARTESIAN_POINT ( 'NONE',  ( -71.80000000218494449, 9.999999999999998224, 17.49999999999999645 ) ) ;
#9290 = ORIENTED_EDGE ( 'NONE', *, *, #12659, .T. ) ;
#9291 = CARTESIAN_POINT ( 'NONE',  ( 52.03124999999999289, 11.24264068711929276, 18.00000000000000355 ) ) ;
#9292 =( LENGTH_UNIT ( ) NAMED_UNIT ( * ) SI_UNIT ( .MILLI., .METRE. ) );
#9293 = CARTESIAN_POINT ( 'NONE',  ( -4.000000000000000000, -1.656854249492383246, -2.512499997268812457 ) ) ;
#9294 = AXIS2_PLACEMENT_3D ( 'NONE', #8721, #17932, #21145 ) ;
#9295 = EDGE_CURVE ( 'NONE', #7848, #20461, #2384, .T. ) ;
#9296 = DIRECTION ( 'NONE',  ( 1.000000000000000000, -0.000000000000000000, -0.000000000000000000 ) ) ;
#9297 = ORIENTED_EDGE ( 'NONE', *, *, #10504, .T. ) ;
#9298 = CARTESIAN_POINT ( 'NONE',  ( -1.656854249492379250, 4.000000000000000000, 18.81250000000001776 ) ) ;
#9299 = DIRECTION ( 'NONE',  ( -0.3420201433256622181, 0.9396926207859106484, 1.232595164407828100E-31 ) ) ;
#9300 = DIRECTION ( 'NONE',  ( 0.000000000000000000, 0.000000000000000000, 1.000000000000000000 ) ) ;
#9301 = ORIENTED_EDGE ( 'NONE', *, *, #10543, .T. ) ;
#9302 = LINE ( 'NONE', #16132, #14912 ) ;
#9303 = DIRECTION ( 'NONE',  ( 0.000000000000000000, 0.000000000000000000, -1.000000000000000000 ) ) ;
#9304 = CARTESIAN_POINT ( 'NONE',  ( 69.79999999999999716, 11.76776695296636888, 13.23223304703362579 ) ) ;
#9305 = DIRECTION ( 'NONE',  ( -1.000000000000000000, -0.000000000000000000, -0.000000000000000000 ) ) ;
#9306 = CYLINDRICAL_SURFACE ( 'NONE', #18722, 8.749000000000002331 ) ;
#9307 = SHAPE_REPRESENTATION ( 'Linear Guide Rail Blocks', ( #7318 ), #14589 ) ;
#9308 = CARTESIAN_POINT ( 'NONE',  ( 50.47106816583844591, 5.971812294485345340, 13.41119689145326710 ) ) ;
#9309 = CARTESIAN_POINT ( 'NONE',  ( 6.353591512924457348E-16, -3.458734125000000326, -1.012499998634402543 ) ) ;
#9310 = CARTESIAN_POINT ( 'NONE',  ( -1.432654583217639166, 3.458734125000000770, 15.50000000136560807 ) ) ;
#9311 = DIRECTION ( 'NONE',  ( 1.000000000000000000, 0.000000000000000000, -1.224646799147353207E-16 ) ) ;
#9312 = DIRECTION ( 'NONE',  ( 1.000000000000000000, 7.703719777548943412E-32, 0.000000000000000000 ) ) ;
#9313 = VERTEX_POINT ( 'NONE', #15004 ) ;
#9314 = CARTESIAN_POINT ( 'NONE',  ( 65.00000000000000000, -15.00000000000000000, 10.00000000000007105 ) ) ;
#9315 = CARTESIAN_POINT ( 'NONE',  ( -60.00000000000000711, 15.00000000000000000, 10.00000000000004974 ) ) ;
#9316 = DIRECTION ( 'NONE',  ( -1.000000000000000000, -0.000000000000000000, -0.000000000000000000 ) ) ;
#9317 = VERTEX_POINT ( 'NONE', #20700 ) ;
#9318 = ORIENTED_EDGE ( 'NONE', *, *, #14039, .T. ) ;
#9319 = DIRECTION ( 'NONE',  ( 0.000000000000000000, 0.000000000000000000, -1.000000000000000000 ) ) ;
#9320 = ORIENTED_EDGE ( 'NONE', *, *, #7147, .F. ) ;
#9321 = CARTESIAN_POINT ( 'NONE',  ( 58.40625000000000711, 13.99999999999999289, 13.34314575050759544 ) ) ;
#9322 = EDGE_LOOP ( 'NONE', ( #9415, #18413, #12386, #787, #4602, #21294 ) ) ;
#9323 = DIRECTION ( 'NONE',  ( -1.000000000000000000, -7.703719777548943412E-32, 0.000000000000000000 ) ) ;
#9324 = ORIENTED_EDGE ( 'NONE', *, *, #20632, .T. ) ;
#9325 = CARTESIAN_POINT ( 'NONE',  ( 54.40856816583843880, 13.97181229448534978, 13.27509460956196641 ) ) ;
#9326 = CIRCLE ( 'NONE', #10486, 4.000000000000001776 ) ;
#9327 = CARTESIAN_POINT ( 'NONE',  ( 71.25000000109248788, 9.999999999999998224, 17.06698730000000097 ) ) ;
#9328 = ADVANCED_FACE ( 'NONE', ( #20458 ), #11277, .T. ) ;
#9329 = CARTESIAN_POINT ( 'NONE',  ( 4.000000000000000888, 1.656854249492381248, 19.56250000000001421 ) ) ;
#9330 = CARTESIAN_POINT ( 'NONE',  ( 71.95000000109247651, 11.46158073645647235, 13.53841926354352232 ) ) ;
#9331 = AXIS2_PLACEMENT_3D ( 'NONE', #11157, #1779, #20092 ) ;
#9332 = PRODUCT_DEFINITION_SHAPE ( 'NONE', 'NONE',  #18958 ) ;
#9333 = ORIENTED_EDGE ( 'NONE', *, *, #5557, .T. ) ;
#9334 = CARTESIAN_POINT ( 'NONE',  ( -1.656854249492379250, 4.000000000000000000, 17.93750000273119483 ) ) ;
#9335 = DIRECTION ( 'NONE',  ( 1.000000000000000000, 7.703719777548943412E-32, 0.000000000000000000 ) ) ;
#9336 = CARTESIAN_POINT ( 'NONE',  ( 59.06250000000000711, 5.999999999999996447, 15.00000000000001599 ) ) ;
#9337 = CARTESIAN_POINT ( 'NONE',  ( -65.00000000000000000, 9.999999999999998224, 14.99999999999999645 ) ) ;
#9338 = EDGE_CURVE ( 'NONE', #16266, #892, #22546, .T. ) ;
#9339 = DIRECTION ( 'NONE',  ( 0.000000000000000000, 0.000000000000000000, 1.000000000000000000 ) ) ;
#9340 = DIRECTION ( 'NONE',  ( -0.5000000000000013323, 0.000000000000000000, 0.8660254037844380415 ) ) ;
#9341 = VECTOR ( 'NONE', #18971, 1000.000000000000000 ) ;
#9342 = CARTESIAN_POINT ( 'NONE',  ( 3.803704290982252711, -5.309483803148803638, -3.700000000000000622 ) ) ;
#9343 = ORIENTED_EDGE ( 'NONE', *, *, #10164, .F. ) ;
#9344 = CARTESIAN_POINT ( 'NONE',  ( 4.000000000000000888, 4.898587196589412829E-16, 18.50000000000001066 ) ) ;
#9345 = CARTESIAN_POINT ( 'NONE',  ( -4.000000000000000000, 0.8576368993457507139, -3.433240632782198709 ) ) ;
#9346 = CARTESIAN_POINT ( 'NONE',  ( 0.000000000000000000, 0.000000000000000000, -5.000000000000000000 ) ) ;
#9347 = VERTEX_POINT ( 'NONE', #4307 ) ;
#9348 = PLANE ( 'NONE',  #5159 ) ;
#9349 = CARTESIAN_POINT ( 'NONE',  ( 70.64999999999999147, 12.50000000000000000, 13.96446609406725692 ) ) ;
#9350 = CARTESIAN_POINT ( 'NONE',  ( 1.799999999999999600, 0.000000000000000000, 0.000000000000000000 ) ) ;
#9351 = DIRECTION ( 'NONE',  ( 0.3420201433256622181, -0.9396926207859107594, 0.000000000000000000 ) ) ;
#9352 = ORIENTED_EDGE ( 'NONE', *, *, #22256, .T. ) ;
#9353 = CARTESIAN_POINT ( 'NONE',  ( 3.679171394226031122, 2.494631558665830973, -0.3503314178412474389 ) ) ;
#9354 = VERTEX_POINT ( 'NONE', #2614 ) ;
#9355 = FACE_OUTER_BOUND ( 'NONE', #6987, .T. ) ;
#9356 = CARTESIAN_POINT ( 'NONE',  ( 1.656854249492381470, 4.000000000000000000, 15.68750000000001066 ) ) ;
#9357 = DIRECTION ( 'NONE',  ( 0.000000000000000000, 0.000000000000000000, -1.000000000000000000 ) ) ;
#9358 = ADVANCED_FACE ( 'NONE', ( #227 ), #4065, .F. ) ;
#9359 = FACE_BOUND ( 'NONE', #17332, .T. ) ;
#9360 = EDGE_CURVE ( 'NONE', #19331, #23136, #18678, .T. ) ;
#9361 = CARTESIAN_POINT ( 'NONE',  ( 2.828427124746191179, 2.828427124746190291, 17.75000000273119483 ) ) ;
#9362 = CARTESIAN_POINT ( 'NONE',  ( 72.25000000109247367, 9.999999999999998224, 17.06698730000000097 ) ) ;
#9363 = VERTEX_POINT ( 'NONE', #9833 ) ;
#9364 = DIRECTION ( 'NONE',  ( 0.000000000000000000, 0.000000000000000000, 1.000000000000000000 ) ) ;
#9365 = DIRECTION ( 'NONE',  ( -0.000000000000000000, -0.000000000000000000, 1.000000000000000000 ) ) ;
#9366 = EDGE_CURVE ( 'NONE', #7146, #3630, #15319, .T. ) ;
#9367 = CARTESIAN_POINT ( 'NONE',  ( 67.05000000109247082, 12.06698730000000097, 14.99999999999999645 ) ) ;
#9368 = CARTESIAN_POINT ( 'NONE',  ( 3.458734125000002102, -1.432654583217639610, 15.87500000136560807 ) ) ;
#9369 = FACE_OUTER_BOUND ( 'NONE', #9159, .T. ) ;
#9370 = AXIS2_PLACEMENT_3D ( 'NONE', #4375, #11713, #20881 ) ;
#9371 = FACE_OUTER_BOUND ( 'NONE', #4461, .T. ) ;
#9372 = CARTESIAN_POINT ( 'NONE',  ( -3.458734125000000770, 1.432654583217640498, -3.074999998634403209 ) ) ;
#9373 = CARTESIAN_POINT ( 'NONE',  ( -68.20000000218495018, 9.999999999999998224, 12.49999999999999289 ) ) ;
#9374 = CARTESIAN_POINT ( 'NONE',  ( -2.445694354108819191, 2.445694354108820523, 13.31250000136560452 ) ) ;
#9375 = CARTESIAN_POINT ( 'NONE',  ( -67.15000000218495302, 7.499999999999996447, 16.03553390593273775 ) ) ;
#9376 = ORIENTED_EDGE ( 'NONE', *, *, #13631, .T. ) ;
#9377 = CARTESIAN_POINT ( 'NONE',  ( -67.80000000109247082, 12.06698729999999919, 14.14382582708705094 ) ) ;
#9378 = ORIENTED_EDGE ( 'NONE', *, *, #10409, .T. ) ;
#9379 = CARTESIAN_POINT ( 'NONE',  ( 57.81018183416157541, 14.00000000000000000, 15.06805114094561304 ) ) ;
#9380 = CARTESIAN_POINT ( 'NONE',  ( -65.75000000109247367, 8.538419263543522320, 16.46158073645647235 ) ) ;
#9381 = CONTEXT_DEPENDENT_SHAPE_REPRESENTATION ( #15316, #16591 ) ;
#9382 = CARTESIAN_POINT ( 'NONE',  ( 17.72176332617111072, 4.729599034760502363, 10.00000000000008882 ) ) ;
#9383 = ORIENTED_EDGE ( 'NONE', *, *, #22864, .T. ) ;
#9384 = EDGE_CURVE ( 'NONE', #18029, #12600, #13093, .T. ) ;
#9385 = VERTEX_POINT ( 'NONE', #19496 ) ;
#9386 = CARTESIAN_POINT ( 'NONE',  ( 3.458734125000002546, -1.432654583217639610, 16.12500000136560629 ) ) ;
#9387 = CARTESIAN_POINT ( 'NONE',  ( 53.90625000000000000, 12.99999999999999645, 13.75735931288070191 ) ) ;
#9388 = AXIS2_PLACEMENT_3D ( 'NONE', #22842, #6454, #3165 ) ;
#9389 = CARTESIAN_POINT ( 'NONE',  ( -70.80000000109248504, 9.143825827087050939, 12.93301269999999370 ) ) ;
#9390 = EDGE_CURVE ( 'NONE', #16438, #14597, #21399, .T. ) ;
#9391 = CARTESIAN_POINT ( 'NONE',  ( -71.05000000109245661, 9.999999999999998224, 12.93301269999999192 ) ) ;
#9392 = CARTESIAN_POINT ( 'NONE',  ( -3.458734124999999437, 1.432654583217640498, 10.62500000136560807 ) ) ;
#9393 = DIRECTION ( 'NONE',  ( 0.000000000000000000, 0.000000000000000000, 1.000000000000000000 ) ) ;
#9394 = EDGE_CURVE ( 'NONE', #15051, #10887, #21157, .T. ) ;
#9395 = CARTESIAN_POINT ( 'NONE',  ( 60.90393183416158962, 13.02818770551463778, 13.82541045382633982 ) ) ;
#9396 = DIRECTION ( 'NONE',  ( -0.000000000000000000, -0.000000000000000000, 1.000000000000000000 ) ) ;
#9397 = EDGE_CURVE ( 'NONE', #22113, #7929, #10077, .T. ) ;
#9398 = FACE_OUTER_BOUND ( 'NONE', #20826, .T. ) ;
#9399 = CARTESIAN_POINT ( 'NONE',  ( -3.458734124999998993, 0.000000000000000000, 10.43750000136560452 ) ) ;
#9400 = CARTESIAN_POINT ( 'NONE',  ( 2.828427124746192067, -2.828427124746189847, 16.50000000273119838 ) ) ;
#9401 = DIRECTION ( 'NONE',  ( 0.000000000000000000, 0.000000000000000000, -1.000000000000000000 ) ) ;
#9402 = VERTEX_POINT ( 'NONE', #19147 ) ;
#9403 = CARTESIAN_POINT ( 'NONE',  ( 70.15000000218495302, 11.03553390593276973, 17.49999999999997158 ) ) ;
#9404 = CARTESIAN_POINT ( 'NONE',  ( 0.000000000000000000, -8.264486777890077462, -4.472189673936873611 ) ) ;
#9405 = VERTEX_POINT ( 'NONE', #17485 ) ;
#9406 = CARTESIAN_POINT ( 'NONE',  ( 56.43750000000000000, 10.00000000000000711, 17.99999999999999645 ) ) ;
#9407 = CIRCLE ( 'NONE', #7504, 5.000000000000011546 ) ;
#9408 = CARTESIAN_POINT ( 'NONE',  ( 3.458734125000000326, 4.235727675282971730E-16, 5.237500001365596347 ) ) ;
#9409 = CIRCLE ( 'NONE', #11335, 0.5000000000000006661 ) ;
#9410 = PLANE ( 'NONE',  #9799 ) ;
#9411 = ORIENTED_EDGE ( 'NONE', *, *, #10808, .T. ) ;
#9412 = CARTESIAN_POINT ( 'NONE',  ( 1.971781867644420635E-15, -4.000000000000000000, 13.25000000000001243 ) ) ;
#9413 = DIRECTION ( 'NONE',  ( 1.000000000000000000, 0.000000000000000000, 0.000000000000000000 ) ) ;
#9414 = CARTESIAN_POINT ( 'NONE',  ( 69.09999999999999432, 12.50000000000000000, 14.99999999999999645 ) ) ;
#9415 = ORIENTED_EDGE ( 'NONE', *, *, #22504, .T. ) ;
#9416 = AXIS2_PLACEMENT_3D ( 'NONE', #19831, #18052, #10657 ) ;
#9417 = FACE_OUTER_BOUND ( 'NONE', #1011, .T. ) ;
#9418 = CARTESIAN_POINT ( 'NONE',  ( -2.117863837641485618E-16, 3.458734125000000770, 0.7375000013655954589 ) ) ;
#9419 = VECTOR ( 'NONE', #6372, 1000.000000000000000 ) ;
#9420 = CARTESIAN_POINT ( 'NONE',  ( 67.14999999999999147, 7.499999999999995559, 13.96446609406725692 ) ) ;
#9421 = ADVANCED_FACE ( 'NONE', ( #3207 ), #1052, .T. ) ;
#9422 = DIRECTION ( 'NONE',  ( 0.3420201433256622736, -0.9396926207859106484, -1.232595164407828100E-31 ) ) ;
#9423 = EDGE_CURVE ( 'NONE', #15256, #10924, #8422, .T. ) ;
#9424 = DIRECTION ( 'NONE',  ( -5.015859645267662560E-17, 0.8191520442889899112, -0.5735764363510487129 ) ) ;
#9425 = CARTESIAN_POINT ( 'NONE',  ( 53.47106816583843880, 5.971812294485345340, 13.41119689145326710 ) ) ;
#9426 = CARTESIAN_POINT ( 'NONE',  ( -3.458734125000000326, 1.432654583217640276, -1.324999998634403653 ) ) ;
#9427 = CARTESIAN_POINT ( 'NONE',  ( -3.458734124999999437, 1.432654583217640498, 13.62500000136560452 ) ) ;
#9428 = CARTESIAN_POINT ( 'NONE',  ( -71.20000000109246230, 12.06698729999999919, 14.14382582708705094 ) ) ;
#9429 = CARTESIAN_POINT ( 'NONE',  ( 1.656854249492381470, 4.000000000000000000, 16.68750000000001066 ) ) ;
#9430 = ORIENTED_EDGE ( 'NONE', *, *, #15710, .F. ) ;
#9431 = CARTESIAN_POINT ( 'NONE',  ( 4.000000000000000888, 4.898587196589412829E-16, 17.50000000000001066 ) ) ;
#9432 = CYLINDRICAL_SURFACE ( 'NONE', #2553, 8.749000000000002331 ) ;
#9433 = DIRECTION ( 'NONE',  ( 0.5000000000000013323, 0.000000000000000000, -0.8660254037844380415 ) ) ;
#9434 = VERTEX_POINT ( 'NONE', #12228 ) ;
#9435 = ORIENTED_EDGE ( 'NONE', *, *, #10609, .T. ) ;
#9436 = DIRECTION ( 'NONE',  ( 1.000000000000000000, 0.000000000000000000, 0.000000000000000000 ) ) ;
#9437 = CARTESIAN_POINT ( 'NONE',  ( 54.75000000000000711, 7.171572875253819923, 17.82842712474619873 ) ) ;
#9438 = ORIENTED_EDGE ( 'NONE', *, *, #18724, .T. ) ;
#9439 = CARTESIAN_POINT ( 'NONE',  ( -6.500000000000002665, -2.517290933526016961, -0.2565799252183981749 ) ) ;
#9440 = ORIENTED_EDGE ( 'NONE', *, *, #1612, .T. ) ;
#9441 = CARTESIAN_POINT ( 'NONE',  ( 54.87731816583843170, 7.123453452023657206, 12.21969229848395599 ) ) ;
#9442 = CARTESIAN_POINT ( 'NONE',  ( 71.90000000109247935, 12.06698730000000275, 15.85617417291294196 ) ) ;
#9443 = LINE ( 'NONE', #7530, #22565 ) ;
#9444 =( BOUNDED_CURVE ( )  B_SPLINE_CURVE ( 2, ( #23130, #10477, #3376, #8908, #19540, #14050, #8549, #17758, #5171 ),
 .UNSPECIFIED., .F., .F. ) 
 B_SPLINE_CURVE_WITH_KNOTS ( ( 3, 2, 2, 2, 3 ),
 ( 0.4500000000000000111, 0.4625000000000000222, 0.4749999999999999778, 0.4874999999999999889, 0.5000000000000000000 ),
 .UNSPECIFIED. ) 
 CURVE ( )  GEOMETRIC_REPRESENTATION_ITEM ( )  RATIONAL_B_SPLINE_CURVE ( ( 1.000000000000000000, 0.9238795325112867385, 1.000000000000000000, 0.9238795325112867385, 1.000000000000000000, 0.9238795325112867385, 1.000000000000000000, 0.9238795325112867385, 1.000000000000000000 ) ) 
 REPRESENTATION_ITEM ( '' )  );
#9445 = CARTESIAN_POINT ( 'NONE',  ( 70.25000000109245946, 9.999999999999998224, 12.93301269999999192 ) ) ;
#9446 = EDGE_LOOP ( 'NONE', ( #6837, #9158 ) ) ;
#9447 = CARTESIAN_POINT ( 'NONE',  ( -1.656854249492379250, 4.000000000000000000, 10.81250000000001243 ) ) ;
#9448 = DIRECTION ( 'NONE',  ( -0.000000000000000000, -0.000000000000000000, 1.000000000000000000 ) ) ;
#9449 = CARTESIAN_POINT ( 'NONE',  ( 54.43518183416157541, 9.931948859054379852, 18.99999999999999289 ) ) ;
#9450 = DIRECTION ( 'NONE',  ( 0.3420201433256622736, -0.9396926207859106484, -1.232595164407828100E-31 ) ) ;
#9451 = CARTESIAN_POINT ( 'NONE',  ( 34.67044344676619971, -9.000000000000003553, 5.000000000000079936 ) ) ;
#9452 = DIRECTION ( 'NONE',  ( 0.000000000000000000, 0.000000000000000000, 1.000000000000000000 ) ) ;
#9453 = CARTESIAN_POINT ( 'NONE',  ( -67.35000000109246798, 11.46158073645647235, 16.46158073645647235 ) ) ;
#9454 = DIRECTION ( 'NONE',  ( 1.000000000000000000, 0.000000000000000000, 0.000000000000000000 ) ) ;
#9455 = VERTEX_POINT ( 'NONE', #2847 ) ;
#9456 = DIRECTION ( 'NONE',  ( -1.000000000000000000, 0.000000000000000000, 0.000000000000000000 ) ) ;
#9457 = CARTESIAN_POINT ( 'NONE',  ( 52.12500000000000711, 12.12132034355964727, 17.12132034355963484 ) ) ;
#9458 = DIRECTION ( 'NONE',  ( -1.000000000000000000, -0.000000000000000000, -0.000000000000000000 ) ) ;
#9459 =( NAMED_UNIT ( * ) SI_UNIT ( $, .STERADIAN. ) SOLID_ANGLE_UNIT ( ) );
#9460 = ORIENTED_EDGE ( 'NONE', *, *, #4072, .T. ) ;
#9461 = EDGE_CURVE ( 'NONE', #15027, #7292, #5016, .T. ) ;
#9462 = FACE_OUTER_BOUND ( 'NONE', #8227, .T. ) ;
#9463 = PLANE ( 'NONE',  #17167 ) ;
#9464 = CARTESIAN_POINT ( 'NONE',  ( 4.211140560182196957, 2.431303136016536470, -3.745885042887433514 ) ) ;
#9465 = CARTESIAN_POINT ( 'NONE',  ( -3.999999999999998224, -1.656854249492383024, 16.18750000273119838 ) ) ;
#9466 = ORIENTED_EDGE ( 'NONE', *, *, #12877, .T. ) ;
#9467 = FACE_OUTER_BOUND ( 'NONE', #15836, .T. ) ;
#9468 = ORIENTED_EDGE ( 'NONE', *, *, #22539, .F. ) ;
#9469 = LINE ( 'NONE', #16767, #10289 ) ;
#9470 = VECTOR ( 'NONE', #6659, 1000.000000000000000 ) ;
#9471 = CARTESIAN_POINT ( 'NONE',  ( -2.828427124746188515, -2.828427124746190735, 13.12500000000001243 ) ) ;
#9472 = DIRECTION ( 'NONE',  ( -1.000000000000000000, -0.000000000000000000, -0.000000000000000000 ) ) ;
#9473 = COLOUR_RGB ( '', 0.40784314, 0.44705882, 0.49803922) ;
#9474 = CARTESIAN_POINT ( 'NONE',  ( 0.5316568767328667677, 7.198601258566900363, -3.296662375310746462 ) ) ;
#9475 = CARTESIAN_POINT ( 'NONE',  ( 70.30000000109247082, 10.85617417291294551, 12.93301269999999192 ) ) ;
#9476 = ORIENTED_EDGE ( 'NONE', *, *, #3933, .T. ) ;
#9477 = AXIS2_PLACEMENT_3D ( 'NONE', #22589, #6192, #11961 ) ;
#9478 = DIRECTION ( 'NONE',  ( 1.000000000000000000, 7.703719777548943412E-32, 0.000000000000000000 ) ) ;
#9479 = CARTESIAN_POINT ( 'NONE',  ( 4.999999999999999112, 0.000000000000000000, 0.000000000000000000 ) ) ;
#9480 = CARTESIAN_POINT ( 'NONE',  ( 66.60000000109248219, 7.933012699999995476, 15.85617417291294196 ) ) ;
#9481 = CARTESIAN_POINT ( 'NONE',  ( -1.432654583217638944, 3.458734125000000326, 18.25000000136560629 ) ) ;
#9482 = DIRECTION ( 'NONE',  ( -0.000000000000000000, 1.000000000000000000, -0.000000000000000000 ) ) ;
#9483 = CARTESIAN_POINT ( 'NONE',  ( -1.432654583217640498, 3.458734125000000770, -3.199999998634403209 ) ) ;
#9484 = CARTESIAN_POINT ( 'NONE',  ( 1.656854249492383024, -3.999999999999999112, 1.612500000000001377 ) ) ;
#9485 = CARTESIAN_POINT ( 'NONE',  ( 9.920644283265380691E-16, 4.000000000000000000, 12.75000000000001066 ) ) ;
#9486 = CARTESIAN_POINT ( 'NONE',  ( -1.432654583217638944, 3.458734125000000326, 13.25000000136560452 ) ) ;
#9487 = CARTESIAN_POINT ( 'NONE',  ( -2.000000000000006661, 3.464101615137750834, 0.000000000000000000 ) ) ;
#9488 = EDGE_LOOP ( 'NONE', ( #6012, #17822, #8021, #22355 ) ) ;
#9489 = CIRCLE ( 'NONE', #12955, 4.250000000000000000 ) ;
#9490 = EDGE_CURVE ( 'NONE', #14307, #669, #6788, .T. ) ;
#9491 = CARTESIAN_POINT ( 'NONE',  ( -69.60000000109248219, 10.85617417291294551, 17.06698730000000097 ) ) ;
#9492 = ORIENTED_EDGE ( 'NONE', *, *, #14521, .T. ) ;
#9493 = CARTESIAN_POINT ( 'NONE',  ( 56.90625000000000711, 13.99999999999999289, 13.34314575050759544 ) ) ;
#9494 = CARTESIAN_POINT ( 'NONE',  ( -69.30000000109247082, 7.933012699999995476, 14.14382582708705094 ) ) ;
#9495 = SHAPE_DEFINITION_REPRESENTATION ( #17381, #20612 ) ;
#9496 = EDGE_CURVE ( 'NONE', #22158, #22026, #15466, .T. ) ;
#9497 = EDGE_LOOP ( 'NONE', ( #557, #23162, #10513, #20689 ) ) ;
#9498 = DIRECTION ( 'NONE',  ( -0.9396926207859107594, -0.3420201433256623291, 1.540743955509804830E-32 ) ) ;
#9499 = ORIENTED_EDGE ( 'NONE', *, *, #4531, .F. ) ;
#9500 = CIRCLE ( 'NONE', #13705, 11.00000000000000000 ) ;
#9501 = AXIS2_PLACEMENT_3D ( 'NONE', #15459, #22366, #17002 ) ;
#9502 = ORIENTED_EDGE ( 'NONE', *, *, #20277, .F. ) ;
#9503 = CARTESIAN_POINT ( 'NONE',  ( -1.432654583217639166, 3.458734125000000770, 15.50000000136560807 ) ) ;
#9504 = EDGE_CURVE ( 'NONE', #21075, #10762, #4958, .T. ) ;
#9505 = CARTESIAN_POINT ( 'NONE',  ( 55.68750000000000000, 9.999999999999989342, 11.99999999999999467 ) ) ;
#9506 = AXIS2_PLACEMENT_3D ( 'NONE', #11077, #9396, #22293 ) ;
#9507 = CARTESIAN_POINT ( 'NONE',  ( -67.95000000109247651, 11.46158073645647235, 16.46158073645647235 ) ) ;
#9508 = CARTESIAN_POINT ( 'NONE',  ( 70.45000000109247651, 9.999999999999998224, 17.06698730000000097 ) ) ;
#9509 = MECHANICAL_DESIGN_GEOMETRIC_PRESENTATION_REPRESENTATION (  '', ( #696 ), #9909 ) ;
#9510 = CARTESIAN_POINT ( 'NONE',  ( -67.50000000109245946, 9.143825827087049163, 17.06698729999999742 ) ) ;
#9511 = CARTESIAN_POINT ( 'NONE',  ( -1.432654583217639832, -3.458734125000000326, 11.87500000136560629 ) ) ;
#9512 = DIRECTION ( 'NONE',  ( -0.000000000000000000, 0.000000000000000000, -1.000000000000000000 ) ) ;
#9513 = CARTESIAN_POINT ( 'NONE',  ( 56.59143183416158962, 11.31069182806491291, 12.02818770551463778 ) ) ;
#9514 = CARTESIAN_POINT ( 'NONE',  ( 71.70000000000000284, 9.999999999999998224, 17.49999999999999645 ) ) ;
#9515 = CONICAL_SURFACE ( 'NONE', #5663, 5.560781378645573980, 1.221730476396046816 ) ;
#9516 = CONICAL_SURFACE ( 'NONE', #22473, 6.500000000000000888, 1.047197551196596521 ) ;
#9517 = PRESENTATION_LAYER_ASSIGNMENT (  '', '', ( #20581 ) ) ;
#9518 = CARTESIAN_POINT ( 'NONE',  ( 55.12500000000000711, 12.12132034355964727, 17.12132034355963484 ) ) ;
#9519 = CARTESIAN_POINT ( 'NONE',  ( 1.872352939448454495E-15, -3.458734125000000326, 10.68750000136560452 ) ) ;
#9520 = CARTESIAN_POINT ( 'NONE',  ( 1.656854249492381470, 4.000000000000000000, 14.81250000273119483 ) ) ;
#9521 = CARTESIAN_POINT ( 'NONE',  ( 2.000000000000000444, 3.464101615137754830, -3.142992957459231018 ) ) ;
#9522 = VERTEX_POINT ( 'NONE', #17718 ) ;
#9523 = CARTESIAN_POINT ( 'NONE',  ( 4.999999999999999112, 8.734705317681626724, 0.4999240074894746311 ) ) ;
#9524 = EDGE_CURVE ( 'NONE', #4420, #13926, #5339, .T. ) ;
#9525 = DIRECTION ( 'NONE',  ( -1.000000000000000000, 0.000000000000000000, 0.000000000000000000 ) ) ;
#9526 = ORIENTED_EDGE ( 'NONE', *, *, #5523, .T. ) ;
#9527 = CARTESIAN_POINT ( 'NONE',  ( 57.06018183416157541, 7.000000000000000000, 14.93194885905437097 ) ) ;
#9528 = CARTESIAN_POINT ( 'NONE',  ( 1.656854249492380360, 4.000000000000000000, -1.887499997268811791 ) ) ;
#9529 = EDGE_CURVE ( 'NONE', #5147, #8640, #22138, .T. ) ;
#9530 = DIRECTION ( 'NONE',  ( 0.9396926207859107594, -0.3420201433256623291, 3.697785493223492838E-32 ) ) ;
#9531 = VERTEX_POINT ( 'NONE', #21045 ) ;
#9532 = CARTESIAN_POINT ( 'NONE',  ( -3.999999999999999112, 1.656854249492380804, 11.93750000000001066 ) ) ;
#9533 = VECTOR ( 'NONE', #13088, 1000.000000000000000 ) ;
#9534 = CARTESIAN_POINT ( 'NONE',  ( 48.67060293033276963, -11.25000000000000355, 5.000000000000079936 ) ) ;
#9535 = LINE ( 'NONE', #9891, #23244 ) ;
#9536 = VERTEX_POINT ( 'NONE', #15813 ) ;
#9537 = EDGE_CURVE ( 'NONE', #7575, #1132, #7558, .T. ) ;
#9538 = PRODUCT_DEFINITION_SHAPE ( 'NONE', 'NONE',  #23698 ) ;
#9539 = EDGE_CURVE ( 'NONE', #10540, #16693, #12814, .T. ) ;
#9540 = CARTESIAN_POINT ( 'NONE',  ( 44.71007725323381976, -9.000000000000003553, 10.29587622221672127 ) ) ;
#9541 = VECTOR ( 'NONE', #13044, 1000.000000000000114 ) ;
#9542 = CARTESIAN_POINT ( 'NONE',  ( 2.445694354108820967, -2.445694354108820079, 1.362500001365595903 ) ) ;
#9543 = CARTESIAN_POINT ( 'NONE',  ( 66.99999999999998579, 8.232233047033627571, 16.76776695296636532 ) ) ;
#9544 = CARTESIAN_POINT ( 'NONE',  ( -1.876855952934450622, 6.421950209808279908, -3.593844378834467612 ) ) ;
#9545 = VECTOR ( 'NONE', #16625, 1000.000000000000000 ) ;
#9546 = CARTESIAN_POINT ( 'NONE',  ( 45.00000000000000000, 2.399706452296379577, 55.00000000000021316 ) ) ;
#9547 = CARTESIAN_POINT ( 'NONE',  ( 54.87731816583843170, 7.123453452023657206, 12.21969229848395599 ) ) ;
#9548 = CARTESIAN_POINT ( 'NONE',  ( 2.445694354108820079, 2.445694354108820523, 4.612500001365595459 ) ) ;
#9549 = CARTESIAN_POINT ( 'NONE',  ( 3.458734125000001658, 4.235727675282972223E-16, 15.18750000136560452 ) ) ;
#9550 = CARTESIAN_POINT ( 'NONE',  ( -20.00000000000001066, 9.999999999999964473, -49.99999999999999289 ) ) ;
#9551 = CARTESIAN_POINT ( 'NONE',  ( -72.05000000109245661, 12.06698730000000097, 14.99999999999999645 ) ) ;
#9552 = COLOUR_RGB ( '', 0.31764706, 0.68627451, 0.89019608) ;
#9553 = DIRECTION ( 'NONE',  ( -0.000000000000000000, -0.000000000000000000, -1.000000000000000000 ) ) ;
#9554 = ORIENTED_EDGE ( 'NONE', *, *, #19677, .T. ) ;
#9555 = LINE ( 'NONE', #20293, #11517 ) ;
#9556 = AXIS2_PLACEMENT_3D ( 'NONE', #21855, #65, #14709 ) ;
#9557 = CARTESIAN_POINT ( 'NONE',  ( 0.3208286057739604957, -4.433571671609698228, -0.3503314178412692548 ) ) ;
#9558 = ADVANCED_FACE ( 'NONE', ( #6941 ), #12585, .F. ) ;
#9559 = CARTESIAN_POINT ( 'NONE',  ( -69.65000000109247935, 9.999999999999998224, 17.06698730000000097 ) ) ;
#9560 = ORIENTED_EDGE ( 'NONE', *, *, #10242, .F. ) ;
#9561 = VERTEX_POINT ( 'NONE', #19726 ) ;
#9562 = CARTESIAN_POINT ( 'NONE',  ( 26.67945438033275707, -11.25000000000000355, 5.000000000000079936 ) ) ;
#9563 = EDGE_CURVE ( 'NONE', #10094, #2131, #1759, .T. ) ;
#9564 = VECTOR ( 'NONE', #19879, 1000.000000000000000 ) ;
#9565 = CARTESIAN_POINT ( 'NONE',  ( 51.28125000000000000, 8.343145750507600766, 11.00000000000000355 ) ) ;
#9566 = ORIENTED_EDGE ( 'NONE', *, *, #18490, .F. ) ;
#9567 = CARTESIAN_POINT ( 'NONE',  ( 0.6640947660595348800, -4.471078309994175548, -3.602146406945708090 ) ) ;
#9568 = ORIENTED_EDGE ( 'NONE', *, *, #13309, .T. ) ;
#9569 = ADVANCED_FACE ( 'NONE', ( #5367 ), #19846, .T. ) ;
#9570 = AXIS2_PLACEMENT_3D ( 'NONE', #10053, #17228, #17343 ) ;
#9571 = UNCERTAINTY_MEASURE_WITH_UNIT (LENGTH_MEASURE( 1.000000000000000082E-05 ), #5510, 'distance_accuracy_value', 'NONE');
#9572 = CARTESIAN_POINT ( 'NONE',  ( 55.72106816583844591, 14.02818770551465377, 16.58880310854672757 ) ) ;
#9573 = CARTESIAN_POINT ( 'NONE',  ( 71.50000000109248788, 7.933012699999995476, 14.14382582708705094 ) ) ;
#9574 = CARTESIAN_POINT ( 'NONE',  ( -3.999999999999999112, 0.000000000000000000, 20.00000000000001066 ) ) ;
#9575 = VECTOR ( 'NONE', #16717, 1000.000000000000000 ) ;
#9576 = CARTESIAN_POINT ( 'NONE',  ( 70.35000000109246798, 11.46158073645647235, 13.53841926354352232 ) ) ;
#9577 = VERTEX_POINT ( 'NONE', #21514 ) ;
#9578 = CARTESIAN_POINT ( 'NONE',  ( 4.000000000000000888, 4.898587196589412829E-16, 13.62500000273119660 ) ) ;
#9579 = CARTESIAN_POINT ( 'NONE',  ( -1.656854249492380582, 4.000000000000000000, 0.2375000027311863493 ) ) ;
#9580 = CARTESIAN_POINT ( 'NONE',  ( 59.90625000000000711, 13.99999999999999289, 13.34314575050759544 ) ) ;
#9581 = CARTESIAN_POINT ( 'NONE',  ( 15.82088754676620823, -9.000000000000005329, 10.00000000000008882 ) ) ;
#9582 = CARTESIAN_POINT ( 'NONE',  ( 69.00000000218494733, 9.999999999999998224, 12.49999999999999289 ) ) ;
#9583 = VECTOR ( 'NONE', #15034, 1000.000000000000000 ) ;
#9584 = CARTESIAN_POINT ( 'NONE',  ( -90.00000000000000000, 0.000000000000000000, 0.000000000000000000 ) ) ;
#9585 = AXIS2_PLACEMENT_3D ( 'NONE', #235, #14888, #1919 ) ;
#9586 = LINE ( 'NONE', #16878, #592 ) ;
#9587 = CARTESIAN_POINT ( 'NONE',  ( 5.432802636760778903, -4.368923434677197903, -3.442664554191212201 ) ) ;
#9588 = ORIENTED_EDGE ( 'NONE', *, *, #18040, .F. ) ;
#9589 = CARTESIAN_POINT ( 'NONE',  ( 52.50000000000000711, 12.12132034355963484, 12.87867965644034740 ) ) ;
#9590 = CARTESIAN_POINT ( 'NONE',  ( 54.99999999999992895, 15.00000000000000000, 1.836970198721037478E-15 ) ) ;
#9591 = CONICAL_SURFACE ( 'NONE', #3818, 2.059999999999998721, 0.9599310885968738161 ) ;
#9592 = ORIENTED_EDGE ( 'NONE', *, *, #14943, .F. ) ;
#9593 = CARTESIAN_POINT ( 'NONE',  ( 0.000000000000000000, -9.680994141368733708, -5.222868219166961978 ) ) ;
#9594 = DIRECTION ( 'NONE',  ( 0.000000000000000000, 0.000000000000000000, 1.000000000000000000 ) ) ;
#9595 = DIRECTION ( 'NONE',  ( -1.000000000000000000, 0.000000000000000000, 0.000000000000000000 ) ) ;
#9596 = AXIS2_PLACEMENT_3D ( 'NONE', #10116, #6269, #11800 ) ;
#9597 = ADVANCED_FACE ( 'NONE', ( #5125 ), #10789, .F. ) ;
#9598 = CARTESIAN_POINT ( 'NONE',  ( -2.449293598294706907E-16, 4.000000000000000000, -2.949999999999997957 ) ) ;
#9599 = EDGE_LOOP ( 'NONE', ( #9181, #21903, #12446, #17382 ) ) ;
#9600 = CARTESIAN_POINT ( 'NONE',  ( -2.449293598294706907E-16, 4.000000000000000000, 1.050000000000000488 ) ) ;
#9601 = ORIENTED_EDGE ( 'NONE', *, *, #19152, .T. ) ;
#9602 = PLANE ( 'NONE',  #11052 ) ;
#9603 =( BOUNDED_CURVE ( )  B_SPLINE_CURVE ( 2, ( #23240, #21553, #8902, #16198, #1207, #6738, #19765, #8434, #17753 ),
 .UNSPECIFIED., .F., .F. ) 
 B_SPLINE_CURVE_WITH_KNOTS ( ( 3, 2, 2, 2, 3 ),
 ( 0.6250000000000005551, 0.6406250000000004441, 0.6562500000000003331, 0.6718750000000002220, 0.6875000000000001110 ),
 .UNSPECIFIED. ) 
 CURVE ( )  GEOMETRIC_REPRESENTATION_ITEM ( )  RATIONAL_B_SPLINE_CURVE ( ( 0.9999999999999973355, 0.9238795325112894030, 1.000000000000000000, 0.9238795325112867385, 1.000000000000000000, 0.9238795325112867385, 1.000000000000000000, 0.9238795325112861834, 1.000000000000000444 ) ) 
 REPRESENTATION_ITEM ( '' )  );
#9604 = CARTESIAN_POINT ( 'NONE',  ( -3.999999999999998224, -1.656854249492383246, 16.06250000000001066 ) ) ;
#9605 = CARTESIAN_POINT ( 'NONE',  ( 1.600000000000004086, 0.000000000000000000, 0.000000000000000000 ) ) ;
#9606 = DIRECTION ( 'NONE',  ( 0.000000000000000000, 0.000000000000000000, -1.000000000000000000 ) ) ;
#9607 = LINE ( 'NONE', #13312, #12931 ) ;
#9608 = CARTESIAN_POINT ( 'NONE',  ( 71.95000000109247651, 11.46158073645647235, 13.53841926354352232 ) ) ;
#9609 = ORIENTED_EDGE ( 'NONE', *, *, #10101, .F. ) ;
#9610 = VECTOR ( 'NONE', #17512, 1000.000000000000000 ) ;
#9611 = LINE ( 'NONE', #19032, #11458 ) ;
#9612 =( GEOMETRIC_REPRESENTATION_CONTEXT ( 3 ) GLOBAL_UNCERTAINTY_ASSIGNED_CONTEXT ( ( #4506 ) ) GLOBAL_UNIT_ASSIGNED_CONTEXT ( ( #7670, #99, #22003 ) ) REPRESENTATION_CONTEXT ( 'NONE', 'WORKASPACE' ) );
#9613 = CARTESIAN_POINT ( 'NONE',  ( 1.799999999999999156, 7.592810154713616459E-16, 6.200000000000021494 ) ) ;
#9614 = CARTESIAN_POINT ( 'NONE',  ( 66.10000000109248219, 10.85617417291294551, 12.93301269999999370 ) ) ;
#9615 = CARTESIAN_POINT ( 'NONE',  ( -2.445694354108818303, -2.445694354108820523, 12.56250000136560629 ) ) ;
#9616 = DIRECTION ( 'NONE',  ( 0.000000000000000000, 0.000000000000000000, 1.000000000000000000 ) ) ;
#9617 = CARTESIAN_POINT ( 'NONE',  ( 2.445694354108820967, -2.445694354108820079, -0.6374999986344023206 ) ) ;
#9618 = CARTESIAN_POINT ( 'NONE',  ( 7.347880794884118750E-16, -4.000000000000000000, 1.550000000000000933 ) ) ;
#9619 = CARTESIAN_POINT ( 'NONE',  ( -71.20000000218495018, 7.499999999999996447, 14.99999999999999645 ) ) ;
#9620 = CARTESIAN_POINT ( 'NONE',  ( -3.458734124999998993, 0.000000000000000000, 13.43750000136560452 ) ) ;
#9621 = CARTESIAN_POINT ( 'NONE',  ( 6.396109596766199168, -9.000000000000005329, 5.000000000000079936 ) ) ;
#9622 = ORIENTED_EDGE ( 'NONE', *, *, #3511, .F. ) ;
#9623 = CARTESIAN_POINT ( 'NONE',  ( -66.20000000109247651, 12.06698729999999919, 14.14382582708705094 ) ) ;
#9624 = VERTEX_POINT ( 'NONE', #23688 ) ;
#9625 = CARTESIAN_POINT ( 'NONE',  ( 56.34375000000000711, 8.343145750507638070, 19.00000000000000711 ) ) ;
#9626 = CARTESIAN_POINT ( 'NONE',  ( -72.25000000109247367, 9.999999999999998224, 17.06698730000000097 ) ) ;
#9627 = CONTEXT_DEPENDENT_SHAPE_REPRESENTATION ( #1344, #5885 ) ;
#9628 = ORIENTED_EDGE ( 'NONE', *, *, #2934, .T. ) ;
#9629 = DIRECTION ( 'NONE',  ( 0.000000000000000000, 0.000000000000000000, -1.000000000000000000 ) ) ;
#9630 = ORIENTED_EDGE ( 'NONE', *, *, #21834, .F. ) ;
#9631 = AXIS2_PLACEMENT_3D ( 'NONE', #11768, #22865, #15477 ) ;
#9632 = ORIENTED_EDGE ( 'NONE', *, *, #6606, .F. ) ;
#9633 = CARTESIAN_POINT ( 'NONE',  ( 3.458734125000001658, 4.235727675282972223E-16, 15.18750000136560452 ) ) ;
#9634 = CARTESIAN_POINT ( 'NONE',  ( 56.90625000000000711, 12.99999999999999645, 13.75735931288070191 ) ) ;
#9635 = CARTESIAN_POINT ( 'NONE',  ( -68.20000000109246230, 7.933012699999995476, 15.85617417291294196 ) ) ;
#9636 = CARTESIAN_POINT ( 'NONE',  ( 67.90000000109247935, 12.06698729999999919, 15.85617417291294196 ) ) ;
#9637 = EDGE_CURVE ( 'NONE', #4680, #12003, #10898, .T. ) ;
#9638 = CARTESIAN_POINT ( 'NONE',  ( -66.20000000109246230, 9.143825827087050939, 12.93301269999999370 ) ) ;
#9639 = CARTESIAN_POINT ( 'NONE',  ( 2.500000000000000000, -1.178949249685214307, 2.042000000000001592 ) ) ;
#9640 = CARTESIAN_POINT ( 'NONE',  ( 58.74768183416157541, 7.830560233210222876, 17.07320092032950498 ) ) ;
#9641 = DIRECTION ( 'NONE',  ( 0.000000000000000000, 0.000000000000000000, 1.000000000000000000 ) ) ;
#9642 = CARTESIAN_POINT ( 'NONE',  ( 1.432654583217640276, 3.458734125000000770, 5.675000001365596347 ) ) ;
#9643 = CARTESIAN_POINT ( 'NONE',  ( 1.025207404391860050E-15, 3.458734125000000326, 10.18750000136560629 ) ) ;
#9644 = CARTESIAN_POINT ( 'NONE',  ( -1.656854249492379250, 4.000000000000000000, 15.93750000273119838 ) ) ;
#9645 = ADVANCED_FACE ( 'NONE', ( #7178 ), #12709, .T. ) ;
#9646 = DIRECTION ( 'NONE',  ( -7.087422195345011518E-32, -1.000000000000000000, -0.000000000000000000 ) ) ;
#9647 = ORIENTED_EDGE ( 'NONE', *, *, #5984, .T. ) ;
#9648 = DIRECTION ( 'NONE',  ( 0.000000000000000000, 0.000000000000000000, 1.000000000000000000 ) ) ;
#9649 = VERTEX_POINT ( 'NONE', #18293 ) ;
#9650 = CARTESIAN_POINT ( 'NONE',  ( 57.81018183416157541, 12.99999999999999822, 15.06805114094562192 ) ) ;
#9651 = SURFACE_STYLE_FILL_AREA ( #4238 ) ;
#9652 = CARTESIAN_POINT ( 'NONE',  ( -3.458734125000000326, 1.432654583217640276, 3.675000001365593238 ) ) ;
#9653 = DIRECTION ( 'NONE',  ( 0.3420201433256622181, -0.9396926207859107594, 0.000000000000000000 ) ) ;
#9654 = ORIENTED_EDGE ( 'NONE', *, *, #16388, .T. ) ;
#9655 = CARTESIAN_POINT ( 'NONE',  ( 1.971781867644420635E-15, -4.000000000000000000, 12.25000000000001066 ) ) ;
#9656 = DIRECTION ( 'NONE',  ( 0.000000000000000000, 0.000000000000000000, 1.000000000000000000 ) ) ;
#9657 = LINE ( 'NONE', #6168, #7975 ) ;
#9658 = ORIENTED_EDGE ( 'NONE', *, *, #7065, .T. ) ;
#9659 = CARTESIAN_POINT ( 'NONE',  ( -70.10000000218494165, 11.76776695296636888, 16.76776695296636532 ) ) ;
#9660 = DIRECTION ( 'NONE',  ( 0.000000000000000000, 0.000000000000000000, 1.000000000000000000 ) ) ;
#9661 = EDGE_CURVE ( 'NONE', #8828, #12158, #14492, .T. ) ;
#9662 = CARTESIAN_POINT ( 'NONE',  ( 1.567478505476134606E-15, 4.618802153517012066, -5.000000000000000000 ) ) ;
#9663 = CARTESIAN_POINT ( 'NONE',  ( 68.99999999999998579, 11.76776695296636888, 13.23223304703362579 ) ) ;
#9664 = ADVANCED_FACE ( 'NONE', ( #14256 ), #20247, .T. ) ;
#9665 = LINE ( 'NONE', #13608, #18093 ) ;
#9666 = DIRECTION ( 'NONE',  ( -1.000000000000000000, -7.703719777548943412E-32, 0.000000000000000000 ) ) ;
#9667 = CARTESIAN_POINT ( 'NONE',  ( 56.18981816583843170, 9.931948859054354983, 11.99999999999999645 ) ) ;
#9668 = CARTESIAN_POINT ( 'NONE',  ( 2.445694354108820967, -2.445694354108820079, 4.362500001365595459 ) ) ;
#9669 = CARTESIAN_POINT ( 'NONE',  ( -3.458734124999998993, -1.432654583217642497, 14.75000000136560452 ) ) ;
#9670 = EDGE_CURVE ( 'NONE', #6426, #11370, #21756, .T. ) ;
#9671 = CARTESIAN_POINT ( 'NONE',  ( -70.85000000109246798, 7.933012699999995476, 14.99999999999999645 ) ) ;
#9672 = CARTESIAN_POINT ( 'NONE',  ( -70.20000000218495018, 9.999999999999998224, 17.49999999999999645 ) ) ;
#9673 = ORIENTED_EDGE ( 'NONE', *, *, #5551, .F. ) ;
#9674 = CARTESIAN_POINT ( 'NONE',  ( 0.02448733951239481094, 4.877042772274728044, -3.751161874094022242 ) ) ;
#9675 = DIRECTION ( 'NONE',  ( 0.000000000000000000, 0.000000000000000000, -1.000000000000000000 ) ) ;
#9676 = CARTESIAN_POINT ( 'NONE',  ( -70.95000000109247651, 11.46158073645647235, 13.53841926354352232 ) ) ;
#9677 = EDGE_LOOP ( 'NONE', ( #9191, #1772, #4978, #8620 ) ) ;
#9678 = ORIENTED_EDGE ( 'NONE', *, *, #20160, .T. ) ;
#9679 = FACE_OUTER_BOUND ( 'NONE', #8526, .T. ) ;
#9680 = CARTESIAN_POINT ( 'NONE',  ( 51.56250000000000711, 5.999999999999996447, 15.00000000000001599 ) ) ;
#9681 = VERTEX_POINT ( 'NONE', #5480 ) ;
#9682 = FACE_OUTER_BOUND ( 'NONE', #18633, .T. ) ;
#9683 = EDGE_CURVE ( 'NONE', #7327, #22486, #23319, .T. ) ;
#9684 = CARTESIAN_POINT ( 'NONE',  ( 70.75000000109247367, 8.538419263543524096, 13.53841926354352054 ) ) ;
#9685 = CARTESIAN_POINT ( 'NONE',  ( -54.99999999999992895, -15.00000000000000000, 5.000000000000015987 ) ) ;
#9686 = CARTESIAN_POINT ( 'NONE',  ( 70.00000000109247367, 7.933012699999995476, 15.85617417291294196 ) ) ;
#9687 = EDGE_CURVE ( 'NONE', #2340, #22874, #5729, .T. ) ;
#9688 = ORIENTED_EDGE ( 'NONE', *, *, #20229, .T. ) ;
#9689 = CARTESIAN_POINT ( 'NONE',  ( -1.656854249492380138, -3.999999999999999112, 12.31250000273119660 ) ) ;
#9690 = LINE ( 'NONE', #672, #338 ) ;
#9691 = CARTESIAN_POINT ( 'NONE',  ( 53.49768183416157541, 12.87654654797631792, 12.21969229848393113 ) ) ;
#9692 = CARTESIAN_POINT ( 'NONE',  ( 71.70000000218495018, 11.76776695296636888, 16.76776695296636532 ) ) ;
#9693 = EDGE_CURVE ( 'NONE', #19458, #13106, #13021, .T. ) ;
#9694 = CARTESIAN_POINT ( 'NONE',  ( -3.458734124999998105, 1.432654583217640276, 17.37500000136560274 ) ) ;
#9695 = FACE_OUTER_BOUND ( 'NONE', #10043, .T. ) ;
#9696 = EDGE_CURVE ( 'NONE', #22762, #9455, #9961, .T. ) ;
#9697 = CARTESIAN_POINT ( 'NONE',  ( -65.85000000109246798, 9.999999999999998224, 17.06698730000000097 ) ) ;
#9698 = CARTESIAN_POINT ( 'NONE',  ( 50.00000000000000000, 15.00000000000003375, 55.00000000000021316 ) ) ;
#9699 = ORIENTED_EDGE ( 'NONE', *, *, #15085, .T. ) ;
#9700 = CARTESIAN_POINT ( 'NONE',  ( -4.000000000000000000, 0.8730739991738342143, -3.223134629628428893 ) ) ;
#9701 = CARTESIAN_POINT ( 'NONE',  ( 36.10423233033275636, -11.25000000000000355, 10.00000000000008882 ) ) ;
#9702 = ORIENTED_EDGE ( 'NONE', *, *, #3203, .T. ) ;
#9703 = VECTOR ( 'NONE', #5737, 1000.000000000000000 ) ;
#9704 = LINE ( 'NONE', #8144, #22746 ) ;
#9705 = CARTESIAN_POINT ( 'NONE',  ( 1.600000000000004086, 0.000000000000000000, 0.000000000000000000 ) ) ;
#9706 = CARTESIAN_POINT ( 'NONE',  ( -3.999999999999999112, 0.000000000000000000, 11.12500000273119660 ) ) ;
#9707 = LINE ( 'NONE', #6218, #4879 ) ;
#9708 = ORIENTED_EDGE ( 'NONE', *, *, #6733, .F. ) ;
#9709 = CARTESIAN_POINT ( 'NONE',  ( 4.999999999999999112, 10.82112760146736363, 1.975651141462276161 ) ) ;
#9710 = ORIENTED_EDGE ( 'NONE', *, *, #14956, .F. ) ;
#9711 = CARTESIAN_POINT ( 'NONE',  ( 4.000000000000000888, 4.898587196589412829E-16, 18.62500000273119483 ) ) ;
#9712 = CARTESIAN_POINT ( 'NONE',  ( -1.656854249492379250, 4.000000000000000000, 15.81250000000001066 ) ) ;
#9713 = FACE_OUTER_BOUND ( 'NONE', #6213, .T. ) ;
#9714 = CARTESIAN_POINT ( 'NONE',  ( 72.50000000000000000, 9.999999999999998224, 14.99999999999999645 ) ) ;
#9715 = CARTESIAN_POINT ( 'NONE',  ( 70.55000000109245661, 11.46158073645647235, 16.46158073645647235 ) ) ;
#9716 = ORIENTED_EDGE ( 'NONE', *, *, #906, .T. ) ;
#9717 = AXIS2_PLACEMENT_3D ( 'NONE', #11702, #6177, #13497 ) ;
#9718 = DIRECTION ( 'NONE',  ( 0.000000000000000000, 0.000000000000000000, -1.000000000000000000 ) ) ;
#9719 = CIRCLE ( 'NONE', #22305, 2.499999999999999556 ) ;
#9720 = DIRECTION ( 'NONE',  ( 0.000000000000000000, 0.000000000000000000, 1.000000000000000000 ) ) ;
#9721 = EDGE_CURVE ( 'NONE', #1063, #6899, #7660, .T. ) ;
#9722 = CARTESIAN_POINT ( 'NONE',  ( 66.00000000109247367, 9.143825827087050939, 12.93301269999999370 ) ) ;
#9723 = CARTESIAN_POINT ( 'NONE',  ( 1.872352939448454495E-15, -3.458734125000000326, 13.68750000136560629 ) ) ;
#9724 = DIRECTION ( 'NONE',  ( 0.3420201433256622736, 0.9396926207859106484, 0.000000000000000000 ) ) ;
#9725 = EDGE_CURVE ( 'NONE', #14838, #2957, #20262, .T. ) ;
#9726 = CARTESIAN_POINT ( 'NONE',  ( -2.117863837641485618E-16, 3.458734125000000770, -2.262499998634403653 ) ) ;
#9727 = CARTESIAN_POINT ( 'NONE',  ( 2.828427124746189847, 2.828427124746190291, 1.925000000000001377 ) ) ;
#9728 = CARTESIAN_POINT ( 'NONE',  ( -4.000000000000000000, -1.656854249492383024, -3.512499997268813345 ) ) ;
#9729 = CARTESIAN_POINT ( 'NONE',  ( 4.999999999999999112, -8.461683424509297780, -2.223716399045659653 ) ) ;
#9730 = LINE ( 'NONE', #4319, #22594 ) ;
#9731 = PRODUCT_DEFINITION_SHAPE ( 'NONE', 'NONE',  #23716 ) ;
#9732 = ORIENTED_EDGE ( 'NONE', *, *, #636, .T. ) ;
#9733 = CARTESIAN_POINT ( 'NONE',  ( -66.05000000109247082, 9.999999999999998224, 12.93301269999999192 ) ) ;
#9734 = VERTEX_POINT ( 'NONE', #9685 ) ;
#9735 = CARTESIAN_POINT ( 'NONE',  ( 55.87500000000000711, 7.171572875253794166, 12.17157287525381726 ) ) ;
#9736 = CARTESIAN_POINT ( 'NONE',  ( -71.15000000109246514, 11.46158073645647235, 13.53841926354352232 ) ) ;
#9737 = PRODUCT_CONTEXT ( 'NONE', #14678, 'mechanical' ) ;
#9738 =( BOUNDED_CURVE ( )  B_SPLINE_CURVE ( 2, ( #4594, #2897, #6633, #21206, #6278, #22905, #9887, #19198, #21095, #13950, #20747, #8445, #4708, #986, #22667, #4821, #17302, #17181, #15404, #10014, #1100, #18844, #4352, #6519, #20861, #10243, #19304, #6163, #22555, #13712, #2430, #12040, #17533, #2783, #17061, #11689, #7964, #15283, #13485, #866, #11932, #10124, #2672, #4467, #2542, #15516, #13839, #22785, #761, #20975, #8093, #11808, #19080, #17417, #6392, #15635, #9034, #8552, #10838, #17878, #21563, #12517, #19657, #6864, #21324, #8793, #7107, #16095, #8914, #6984, #16327, #1452, #23493, #3258, #23382, #21447, #23620, #12279, #19900, #17998, #3502, #1576, #5299, #8671, #17763, #14550, #5059, #12392, #14424 ),
 .UNSPECIFIED., .F., .F. ) 
 B_SPLINE_CURVE_WITH_KNOTS ( ( 3, 2, 2, 2, 2, 2, 2, 2, 2, 2, 2, 2, 2, 2, 2, 2, 2, 2, 2, 2, 2, 2, 2, 2, 2, 2, 2, 2, 2, 2, 2, 2, 2, 2, 2, 2, 2, 2, 2, 2, 2, 2, 2, 2, 3 ),
 ( 0.3697128431780269953, 0.3750000000000000000, 0.3875000000000000111, 0.4000000000000000222, 0.4124999999999999778, 0.4249999999999999889, 0.4375000000000000000, 0.4500000000000000111, 0.4625000000000000222, 0.4749999999999999778, 0.4874999999999999889, 0.5000000000000000000, 0.5124999999999999556, 0.5250000000000000222, 0.5374999999999999778, 0.5500000000000000444, 0.5625000000000000000, 0.5749999999999999556, 0.5875000000000000222, 0.5999999999999999778, 0.6125000000000000444, 0.6250000000000000000, 0.6374999999999999556, 0.6500000000000000222, 0.6624999999999999778, 0.6750000000000000444, 0.6875000000000000000, 0.6999999999999999556, 0.7125000000000000222, 0.7249999999999999778, 0.7375000000000000444, 0.7500000000000000000, 0.7624999999999999556, 0.7750000000000000222, 0.7874999999999999778, 0.8000000000000000444, 0.8125000000000000000, 0.8249999999999999556, 0.8375000000000000222, 0.8499999999999999778, 0.8625000000000000444, 0.8750000000000000000, 0.8874999999999999556, 0.9000000000000000222, 0.9033987602710955578 ),
 .UNSPECIFIED. ) 
 CURVE ( )  GEOMETRIC_REPRESENTATION_ITEM ( )  RATIONAL_B_SPLINE_CURVE ( ( 0.9628430465414361539, 0.9678031320820220662, 1.000000000000000000, 0.9238795325112867385, 1.000000000000000000, 0.9238795325112867385, 1.000000000000000000, 0.9238795325112867385, 1.000000000000000000, 0.9238795325112867385, 1.000000000000000000, 0.9238795325112867385, 1.000000000000000000, 0.9238795325112867385, 1.000000000000000000, 0.9238795325112867385, 1.000000000000000000, 0.9238795325112867385, 1.000000000000000000, 0.9238795325112867385, 1.000000000000000000, 0.9238795325112867385, 1.000000000000000000, 0.9238795325112867385, 1.000000000000000000, 0.9238795325112867385, 1.000000000000000000, 0.9238795325112867385, 1.000000000000000000, 0.9238795325112867385, 1.000000000000000000, 0.9238795325112867385, 1.000000000000000000, 0.9238795325112867385, 1.000000000000000000, 0.9238795325112867385, 1.000000000000000000, 0.9238795325112867385, 1.000000000000000000, 0.9238795325112867385, 1.000000000000000000, 0.9238795325112867385, 1.000000000000000000, 0.9238795325112867385, 1.000000000000000000, 0.9238795325112867385, 1.000000000000000000, 0.9238795325112867385, 1.000000000000000000, 0.9238795325112867385, 1.000000000000000000, 0.9238795325112867385, 1.000000000000000000, 0.9238795325112867385, 1.000000000000000000, 0.9238795325112867385, 1.000000000000000000, 0.9238795325112867385, 1.000000000000000000, 0.9238795325112867385, 1.000000000000000000, 0.9238795325112867385, 1.000000000000000000, 0.9238795325112867385, 1.000000000000000000, 0.9238795325112867385, 1.000000000000000000, 0.9238795325112867385, 1.000000000000000000, 0.9238795325112867385, 1.000000000000000000, 0.9238795325112867385, 1.000000000000000000, 0.9238795325112867385, 1.000000000000000000, 0.9238795325112867385, 1.000000000000000000, 0.9238795325112867385, 1.000000000000000000, 0.9238795325112867385, 1.000000000000000000, 0.9238795325112867385, 1.000000000000000000, 0.9238795325112867385, 1.000000000000000000, 0.9238795325112867385, 1.000000000000000000, 0.9793027823425712874, 0.9698607456605483623 ) ) 
 REPRESENTATION_ITEM ( '' )  );
#9739 = VERTEX_POINT ( 'NONE', #6073 ) ;
#9740 = CARTESIAN_POINT ( 'NONE',  ( -4.000000000000000000, 0.000000000000000000, -1.574999997268811569 ) ) ;
#9741 = ORIENTED_EDGE ( 'NONE', *, *, #5989, .F. ) ;
#9742 = EDGE_LOOP ( 'NONE', ( #100, #9062, #2641, #131 ) ) ;
#9743 = CARTESIAN_POINT ( 'NONE',  ( -2.445694354108819191, 2.445694354108820523, 16.56250000136560629 ) ) ;
#9744 = CARTESIAN_POINT ( 'NONE',  ( 56.81250000000000000, 13.00000000000000000, 14.99999999999998757 ) ) ;
#9745 = CARTESIAN_POINT ( 'NONE',  ( -66.35000000109248219, 11.46158073645647235, 16.46158073645647235 ) ) ;
#9746 = CARTESIAN_POINT ( 'NONE',  ( 68.95000000109247651, 8.538419263543522320, 16.46158073645647235 ) ) ;
#9747 = CARTESIAN_POINT ( 'NONE',  ( -66.55000000109247082, 11.46158073645647235, 16.46158073645647235 ) ) ;
#9748 = CARTESIAN_POINT ( 'NONE',  ( -71.54999999999998295, 12.50000000000000000, 16.03553390593273775 ) ) ;
#9749 = CARTESIAN_POINT ( 'NONE',  ( 54.43518183416157541, 9.931948859054372747, 17.99999999999999645 ) ) ;
#9750 = CARTESIAN_POINT ( 'NONE',  ( 72.15000000109247935, 9.999999999999998224, 17.06698730000000097 ) ) ;
#9751 = CARTESIAN_POINT ( 'NONE',  ( -3.458734125000000770, 0.000000000000000000, 1.987500001365596569 ) ) ;
#9752 = CARTESIAN_POINT ( 'NONE',  ( -1.432654583217639610, -3.458734124999999882, 10.62500000136560452 ) ) ;
#9753 = CARTESIAN_POINT ( 'NONE',  ( 4.000000000000000888, 1.656854249492381248, 13.68750000273119483 ) ) ;
#9754 = DIRECTION ( 'NONE',  ( 0.000000000000000000, 0.000000000000000000, -1.000000000000000000 ) ) ;
#9755 = ORIENTED_EDGE ( 'NONE', *, *, #22909, .F. ) ;
#9756 = CYLINDRICAL_SURFACE ( 'NONE', #10527, 4.999999999999997335 ) ;
#9757 = ORIENTED_EDGE ( 'NONE', *, *, #22047, .F. ) ;
#9758 = CARTESIAN_POINT ( 'NONE',  ( 60.24768183416157541, 7.830560233210222876, 17.07320092032950498 ) ) ;
#9759 = CARTESIAN_POINT ( 'NONE',  ( -2.117863837641485618E-16, 3.458734125000000326, 1.487500001365596125 ) ) ;
#9760 = PRODUCT_DEFINITION ( 'UNKNOWN', '', #4180, #439 ) ;
#9761 = PLANE ( 'NONE',  #8647 ) ;
#9762 = ORIENTED_EDGE ( 'NONE', *, *, #10292, .T. ) ;
#9763 = AXIS2_PLACEMENT_3D ( 'NONE', #3550, #9316, #22085 ) ;
#9764 = CARTESIAN_POINT ( 'NONE',  ( -2.828427124746189403, 2.828427124746190291, 12.87500000000001066 ) ) ;
#9765 = ADVANCED_FACE ( 'NONE', ( #18522 ), #14846, .F. ) ;
#9766 = VECTOR ( 'NONE', #9340, 999.9999999999997726 ) ;
#9767 = CARTESIAN_POINT ( 'NONE',  ( 0.000000000000000000, 0.000000000000000000, -5.000000000000000888 ) ) ;
#9768 = VERTEX_POINT ( 'NONE', #18773 ) ;
#9769 =( BOUNDED_CURVE ( )  B_SPLINE_CURVE ( 2, ( #18243, #9403, #5795, #21836, #21941, #20268, #5550, #11085, #5437 ),
 .UNSPECIFIED., .F., .F. ) 
 B_SPLINE_CURVE_WITH_KNOTS ( ( 3, 2, 2, 2, 3 ),
 ( 0.2500000000000006661, 0.2656250000000005551, 0.2812500000000004441, 0.2968750000000003886, 0.3125000000000002776 ),
 .UNSPECIFIED. ) 
 CURVE ( )  GEOMETRIC_REPRESENTATION_ITEM ( )  RATIONAL_B_SPLINE_CURVE ( ( 0.9999999999999967804, 0.9238795325112899581, 1.000000000000000000, 0.9238795325112867385, 1.000000000000000000, 0.9238795325112867385, 1.000000000000000000, 0.9238795325112854062, 1.000000000000001332 ) ) 
 REPRESENTATION_ITEM ( '' )  );
#9770 = CARTESIAN_POINT ( 'NONE',  ( -71.10000000218494165, 8.232233047033627571, 16.76776695296636532 ) ) ;
#9771 = DIRECTION ( 'NONE',  ( -0.9396926207859138680, 0.000000000000000000, -0.3420201433256536139 ) ) ;
#9772 = CARTESIAN_POINT ( 'NONE',  ( -4.024497503033519941, -2.323544716729390558, -3.572167766733381544 ) ) ;
#9773 = CARTESIAN_POINT ( 'NONE',  ( 4.999999999999999112, 1.239665997526886665, 9.314797388894895391 ) ) ;
#9774 = B_SPLINE_CURVE_WITH_KNOTS ( 'NONE', 1,
 ( #5918, #16471 ),
 .UNSPECIFIED., .F., .F.,
 ( 2, 2 ),
 ( 0.000000000000000000, 1.000000000000000000 ),
 .UNSPECIFIED. ) ;
#9775 = CARTESIAN_POINT ( 'NONE',  ( 27.56832511966726784, -11.25000000000000355, 5.000000000000079936 ) ) ;
#9776 = CARTESIAN_POINT ( 'NONE',  ( 70.80000000109248504, 9.143825827087050939, 12.93301269999999370 ) ) ;
#9778 = CARTESIAN_POINT ( 'NONE',  ( -66.90000000000000568, 9.999999999999998224, 17.49999999999999645 ) ) ;
#9777 = AXIS2_PLACEMENT_3D ( 'NONE', #5143, #23467, #7074 ) ;
#9779 = CARTESIAN_POINT ( 'NONE',  ( 54.87731816583843170, 7.830560233210212218, 12.92679907967049679 ) ) ;
#9780 = AXIS2_PLACEMENT_3D ( 'NONE', #20794, #2243, #9935 ) ;
#9781 = CARTESIAN_POINT ( 'NONE',  ( -1.432654583217640942, -3.458734124999999882, -2.074999998634404097 ) ) ;
#9782 = CARTESIAN_POINT ( 'NONE',  ( 1.872352939448454495E-15, -3.458734125000000770, 13.93750000136560629 ) ) ;
#9783 = CARTESIAN_POINT ( 'NONE',  ( -14.98942794071655271, -8.974600000000002353, 5.000000000000079936 ) ) ;
#9784 = CARTESIAN_POINT ( 'NONE',  ( -70.25000000109245946, 9.999999999999998224, 12.93301269999999192 ) ) ;
#9785 = CARTESIAN_POINT ( 'NONE',  ( -2.449293598294706907E-16, 4.000000000000000000, -1.949999999999998623 ) ) ;
#9786 = ORIENTED_EDGE ( 'NONE', *, *, #23599, .F. ) ;
#9787 = DIRECTION ( 'NONE',  ( -1.000000000000000000, -0.000000000000000000, -0.000000000000000000 ) ) ;
#9788 = CARTESIAN_POINT ( 'NONE',  ( 2.828427124746189847, 2.828427124746190291, 4.050000002731186655 ) ) ;
#9789 = CARTESIAN_POINT ( 'NONE',  ( -71.05000000109247082, 12.06698730000000097, 14.99999999999999645 ) ) ;
#9790 = ORIENTED_EDGE ( 'NONE', *, *, #18323, .F. ) ;
#9791 = ORIENTED_EDGE ( 'NONE', *, *, #20632, .F. ) ;
#9792 = EDGE_CURVE ( 'NONE', #14716, #5267, #17609, .T. ) ;
#9793 = CARTESIAN_POINT ( 'NONE',  ( -4.000000000000000000, 0.000000000000000000, 1.425000002731187765 ) ) ;
#9794 = EDGE_CURVE ( 'NONE', #12677, #3140, #13405, .T. ) ;
#9795 = CARTESIAN_POINT ( 'NONE',  ( 52.96875000000000000, 5.999999999999987566, 13.34314575050763452 ) ) ;
#9796 = EDGE_LOOP ( 'NONE', ( #19107, #13340, #1196, #10839 ) ) ;
#9797 = CARTESIAN_POINT ( 'NONE',  ( -10.00000000000000000, 0.000000000000000000, 0.000000000000000000 ) ) ;
#9798 = UNCERTAINTY_MEASURE_WITH_UNIT (LENGTH_MEASURE( 1.000000000000000082E-05 ), #11687, 'distance_accuracy_value', 'NONE');
#9799 = AXIS2_PLACEMENT_3D ( 'NONE', #11336, #9530, #21946 ) ;
#9800 = CIRCLE ( 'NONE', #17060, 2.500000000000000888 ) ;
#9801 = EDGE_CURVE ( 'NONE', #2890, #2006, #10360, .T. ) ;
#9802 = CARTESIAN_POINT ( 'NONE',  ( 69.30000000109247082, 10.85617417291294551, 12.93301269999999370 ) ) ;
#9803 = CARTESIAN_POINT ( 'NONE',  ( 69.80000000109247082, 10.85617417291294551, 17.06698729999999742 ) ) ;
#9804 = VERTEX_POINT ( 'NONE', #199 ) ;
#9805 = CONICAL_SURFACE ( 'NONE', #9043, 4.000000000000000000, 0.8911886515913786111 ) ;
#9806 = CARTESIAN_POINT ( 'NONE',  ( 4.000000000000000000, 4.898587196589412829E-16, -0.07499999726881187434 ) ) ;
#9807 = CARTESIAN_POINT ( 'NONE',  ( 58.50000000000000000, 12.82842712474617741, 12.17157287525379239 ) ) ;
#9808 = DIRECTION ( 'NONE',  ( -1.000000000000000000, 0.000000000000000000, 0.000000000000000000 ) ) ;
#9809 = CARTESIAN_POINT ( 'NONE',  ( 1.432654583217641164, 3.458734125000000326, 19.12500000136560629 ) ) ;
#9810 = CARTESIAN_POINT ( 'NONE',  ( 34.99999999999999289, 1.500000000000009992, -50.00000000000000711 ) ) ;
#9811 = CARTESIAN_POINT ( 'NONE',  ( -66.55000000109247082, 11.46158073645647235, 16.46158073645647235 ) ) ;
#9812 = ORIENTED_EDGE ( 'NONE', *, *, #19903, .F. ) ;
#9813 = DIRECTION ( 'NONE',  ( -1.000000000000000000, -0.000000000000000000, -0.000000000000000000 ) ) ;
#9814 = ORIENTED_EDGE ( 'NONE', *, *, #20323, .F. ) ;
#9815 = DIRECTION ( 'NONE',  ( -1.000000000000000000, -7.703719777548943412E-32, 0.000000000000000000 ) ) ;
#9816 = EDGE_CURVE ( 'NONE', #7712, #17107, #9443, .T. ) ;
#9817 = CARTESIAN_POINT ( 'NONE',  ( -70.79999999999999716, 11.76776695296636888, 16.76776695296636532 ) ) ;
#9818 = ORIENTED_EDGE ( 'NONE', *, *, #22022, .T. ) ;
#9819 = CARTESIAN_POINT ( 'NONE',  ( 4.000000000000000000, 2.309401076758497151, -3.433295621305379353 ) ) ;
#9820 = EDGE_CURVE ( 'NONE', #14005, #19193, #1847, .T. ) ;
#9821 = LINE ( 'NONE', #4881, #6065 ) ;
#9822 = DIRECTION ( 'NONE',  ( 0.000000000000000000, 0.000000000000000000, -1.000000000000000000 ) ) ;
#9823 = EDGE_CURVE ( 'NONE', #14025, #14210, #14780, .T. ) ;
#9824 = CARTESIAN_POINT ( 'NONE',  ( 71.30000000218494449, 8.232233047033629347, 13.23223304703362402 ) ) ;
#9825 = EDGE_LOOP ( 'NONE', ( #9502, #7998, #2097, #23401 ) ) ;
#9826 = FACE_OUTER_BOUND ( 'NONE', #2038, .T. ) ;
#9827 = ORIENTED_EDGE ( 'NONE', *, *, #20775, .T. ) ;
#9828 = CARTESIAN_POINT ( 'NONE',  ( 71.90000000109247935, 12.06698729999999919, 15.85617417291294196 ) ) ;
#9829 = CARTESIAN_POINT ( 'NONE',  ( -3.999999999999999112, 0.000000000000000000, 15.00000000000001066 ) ) ;
#9830 = EDGE_CURVE ( 'NONE', #9402, #21235, #16979, .T. ) ;
#9831 = CARTESIAN_POINT ( 'NONE',  ( 71.75000000218496155, 11.03553390593273598, 17.50000000000000355 ) ) ;
#9832 = ADVANCED_FACE ( 'NONE', ( #4154 ), #16307, .T. ) ;
#9833 = CARTESIAN_POINT ( 'NONE',  ( -20.00005079999999680, 4.898587196589412829E-16, -4.000000000000000000 ) ) ;
#9834 = DIRECTION ( 'NONE',  ( -1.000000000000000000, 0.000000000000000000, 0.000000000000000000 ) ) ;
#9835 = CARTESIAN_POINT ( 'NONE',  ( 70.70000000109247651, 9.143825827087049163, 17.06698730000000097 ) ) ;
#9836 = ORIENTED_EDGE ( 'NONE', *, *, #2170, .T. ) ;
#9837 = DIRECTION ( 'NONE',  ( 0.000000000000000000, 0.9510565162951521989, 0.3090169943749515591 ) ) ;
#9838 = CARTESIAN_POINT ( 'NONE',  ( -2.828427124746188515, -2.828427124746190735, 10.25000000273119660 ) ) ;
#9839 = CARTESIAN_POINT ( 'NONE',  ( 68.80000000109247082, 12.06698730000000275, 14.14382582708705094 ) ) ;
#9840 = CARTESIAN_POINT ( 'NONE',  ( -2.445694354108818303, -2.445694354108820523, 13.56250000136560629 ) ) ;
#9841 = FACE_OUTER_BOUND ( 'NONE', #1666, .T. ) ;
#9842 = CARTESIAN_POINT ( 'NONE',  ( 4.999999999999999112, -4.472189673936844301, 8.264486777890091673 ) ) ;
#9843 = VERTEX_POINT ( 'NONE', #23148 ) ;
#9844 = CARTESIAN_POINT ( 'NONE',  ( -4.000000000000000000, 0.000000000000000000, 3.300000000000002487 ) ) ;
#9845 = DIRECTION ( 'NONE',  ( 0.3420201433256622181, -0.9396926207859107594, 0.000000000000000000 ) ) ;
#9846 = DIRECTION ( 'NONE',  ( 1.000000000000000000, 0.000000000000000000, 0.000000000000000000 ) ) ;
#9847 = DIRECTION ( 'NONE',  ( 0.000000000000000000, 0.000000000000000000, 1.000000000000000000 ) ) ;
#9848 = ORIENTED_EDGE ( 'NONE', *, *, #18165, .T. ) ;
#9849 = CARTESIAN_POINT ( 'NONE',  ( -66.55000000109247082, 8.538419263543522320, 16.46158073645647235 ) ) ;
#9850 = ORIENTED_EDGE ( 'NONE', *, *, #1837, .T. ) ;
#9851 = VECTOR ( 'NONE', #16424, 1000.000000000000000 ) ;
#9852 = CARTESIAN_POINT ( 'NONE',  ( 59.43750000000000711, 10.00000000000001776, 18.99999999999999645 ) ) ;
#9853 = CARTESIAN_POINT ( 'NONE',  ( -68.55000000109247082, 8.538419263543524096, 13.53841926354352054 ) ) ;
#9854 = EDGE_CURVE ( 'NONE', #9739, #20452, #22853, .T. ) ;
#9855 = EDGE_LOOP ( 'NONE', ( #5779, #19625 ) ) ;
#9856 = LINE ( 'NONE', #4212, #9419 ) ;
#9857 = ORIENTED_EDGE ( 'NONE', *, *, #14069, .F. ) ;
#9858 = EDGE_CURVE ( 'NONE', #19131, #13175, #14200, .T. ) ;
#9859 = ORIENTED_EDGE ( 'NONE', *, *, #7673, .T. ) ;
#9860 = CARTESIAN_POINT ( 'NONE',  ( 1.432654583217641386, 3.458734125000000770, 18.37500000136560274 ) ) ;
#9861 = EDGE_CURVE ( 'NONE', #18272, #21915, #3060, .T. ) ;
#9862 = CARTESIAN_POINT ( 'NONE',  ( 56.06250000000000000, 6.999999999999997335, 15.00000000000000533 ) ) ;
#9863 = VECTOR ( 'NONE', #11520, 1000.000000000000114 ) ;
#9864 = CIRCLE ( 'NONE', #267, 4.000000000000001776 ) ;
#9865 = EDGE_CURVE ( 'NONE', #12130, #16102, #17890, .T. ) ;
#9866 = CARTESIAN_POINT ( 'NONE',  ( -68.50000000109247367, 10.85617417291294551, 12.93301269999999370 ) ) ;
#9867 = CARTESIAN_POINT ( 'NONE',  ( 68.30000000109247082, 7.933012699999995476, 14.14382582708705094 ) ) ;
#9868 = CARTESIAN_POINT ( 'NONE',  ( -67.30000000109247082, 12.06698730000000275, 15.85617417291294196 ) ) ;
#9869 = CARTESIAN_POINT ( 'NONE',  ( 40.95362874676621345, -9.000000000000005329, 5.000000000000079936 ) ) ;
#9870 = CARTESIAN_POINT ( 'NONE',  ( 59.12268183416157541, 12.07320092032950676, 17.16943976678977180 ) ) ;
#9871 = DIRECTION ( 'NONE',  ( 0.000000000000000000, 0.9510565162951544194, -0.3090169943749447312 ) ) ;
#9872 = VECTOR ( 'NONE', #13958, 1000.000000000000000 ) ;
#9873 =( BOUNDED_CURVE ( )  B_SPLINE_CURVE ( 2, ( #10555, #16392, #85, #12465, #12348, #3675, #12817, #17829, #1396 ),
 .UNSPECIFIED., .F., .F. ) 
 B_SPLINE_CURVE_WITH_KNOTS ( ( 3, 2, 2, 2, 3 ),
 ( 0.6500000000000000222, 0.6624999999999999778, 0.6750000000000000444, 0.6875000000000000000, 0.6999999999999999556 ),
 .UNSPECIFIED. ) 
 CURVE ( )  GEOMETRIC_REPRESENTATION_ITEM ( )  RATIONAL_B_SPLINE_CURVE ( ( 1.000000000000000000, 0.9238795325112867385, 1.000000000000000000, 0.9238795325112867385, 1.000000000000000000, 0.9238795325112867385, 1.000000000000000000, 0.9238795325112867385, 1.000000000000000000 ) ) 
 REPRESENTATION_ITEM ( '' )  );
#9874 = CARTESIAN_POINT ( 'NONE',  ( -3.458734125000000326, -1.432654583217642497, 4.050000001365596347 ) ) ;
#9875 = CARTESIAN_POINT ( 'NONE',  ( 1.872352939448454495E-15, -3.458734125000000326, 12.68750000136560629 ) ) ;
#9876 = CARTESIAN_POINT ( 'NONE',  ( 1.971781867644420635E-15, -4.000000000000000000, 11.37500000273119660 ) ) ;
#9877 = B_SPLINE_CURVE_WITH_KNOTS ( 'NONE', 3,
 ( #21729, #3540, #14820, #14946, #9544, #10875, #20044, #1735 ),
 .UNSPECIFIED., .F., .F.,
 ( 4, 2, 2, 4 ),
 ( 0.003797433802554438069, 0.004743183970586236156, 0.005688934138618034243, 0.007580434474681629550 ),
 .UNSPECIFIED. ) ;
#9878 = PLANE ( 'NONE',  #16469 ) ;
#9879 = CIRCLE ( 'NONE', #14461, 8.749000000000002331 ) ;
#9880 = VECTOR ( 'NONE', #13274, 1000.000000000000000 ) ;
#9881 = ORIENTED_EDGE ( 'NONE', *, *, #7673, .F. ) ;
#9882 = CARTESIAN_POINT ( 'NONE',  ( 0.000000000000000000, 0.000000000000000000, 19.04999999999996874 ) ) ;
#9883 = ORIENTED_EDGE ( 'NONE', *, *, #17251, .F. ) ;
#9884 = CARTESIAN_POINT ( 'NONE',  ( 55.84143183416158251, 8.689308171935088865, 17.97181229448535689 ) ) ;
#9885 =( LENGTH_UNIT ( ) NAMED_UNIT ( * ) SI_UNIT ( .MILLI., .METRE. ) );
#9886 = CARTESIAN_POINT ( 'NONE',  ( 1.432654583217642275, -3.458734124999999437, 2.050000001365597679 ) ) ;
#9887 = CARTESIAN_POINT ( 'NONE',  ( -3.458734125000000326, 0.000000000000000000, 1.737500001365596347 ) ) ;
#9888 = ORIENTED_EDGE ( 'NONE', *, *, #12319, .T. ) ;
#9889 = CARTESIAN_POINT ( 'NONE',  ( -2.828427124746189403, 2.828427124746190291, 14.87500000000000888 ) ) ;
#9890 = SURFACE_SIDE_STYLE ('',( #989 ) ) ;
#9891 = CARTESIAN_POINT ( 'NONE',  ( -4.000000000000000000, 4.898587196589412829E-16, 19.04999999999996874 ) ) ;
#9892 = VERTEX_POINT ( 'NONE', #6998 ) ;
#9893 = ADVANCED_FACE ( 'NONE', ( #21576 ), #18014, .T. ) ;
#9894 = AXIS2_PLACEMENT_3D ( 'NONE', #18206, #12370, #17971 ) ;
#9895 = CARTESIAN_POINT ( 'NONE',  ( -71.55000000218494449, 12.50000000000000000, 13.96446609406725869 ) ) ;
#9896 = CARTESIAN_POINT ( 'NONE',  ( 1.432654583217640276, 3.458734125000000770, -2.324999998634404097 ) ) ;
#9897 = CIRCLE ( 'NONE', #11429, 4.000000000000002665 ) ;
#9898 = STYLED_ITEM ( 'NONE', ( #4355 ), #6915 ) ;
#9899 = DIRECTION ( 'NONE',  ( -0.000000000000000000, -0.000000000000000000, -1.000000000000000000 ) ) ;
#9900 =( GEOMETRIC_REPRESENTATION_CONTEXT ( 3 ) GLOBAL_UNCERTAINTY_ASSIGNED_CONTEXT ( ( #15324 ) ) GLOBAL_UNIT_ASSIGNED_CONTEXT ( ( #9885, #7490, #17058 ) ) REPRESENTATION_CONTEXT ( 'NONE', 'WORKASPACE' ) );
#9901 = CARTESIAN_POINT ( 'NONE',  ( 1.025207404391860050E-15, 3.458734125000000770, 18.43750000136560629 ) ) ;
#9902 = CARTESIAN_POINT ( 'NONE',  ( 1.656854249492384135, -3.999999999999999112, 11.31250000000001066 ) ) ;
#9903 = CARTESIAN_POINT ( 'NONE',  ( 69.10000000109248219, 7.933012699999995476, 14.14382582708705094 ) ) ;
#9904 = CARTESIAN_POINT ( 'NONE',  ( -13.27237933033274153, -11.25000000000000355, 5.000000000000079936 ) ) ;
#9905 = CARTESIAN_POINT ( 'NONE',  ( 56.28356816583844591, 8.689308171935074654, 12.02818770551464489 ) ) ;
#9906 = CARTESIAN_POINT ( 'NONE',  ( 1.432654583217640276, 3.458734125000000770, 5.675000001365596347 ) ) ;
#9907 = CARTESIAN_POINT ( 'NONE',  ( -2.445694354108819191, 2.445694354108820523, 11.56250000136560629 ) ) ;
#9908 = DIRECTION ( 'NONE',  ( 7.010384997569516610E-32, 1.000000000000000000, -3.469446951953615175E-16 ) ) ;
#9909 =( GEOMETRIC_REPRESENTATION_CONTEXT ( 3 ) GLOBAL_UNCERTAINTY_ASSIGNED_CONTEXT ( ( #9571 ) ) GLOBAL_UNIT_ASSIGNED_CONTEXT ( ( #5510, #114, #21793 ) ) REPRESENTATION_CONTEXT ( 'NONE', 'WORKASPACE' ) );
#9910 = CARTESIAN_POINT ( 'NONE',  ( -18.72738675928344065, -8.974600000000002353, 10.00000000000008882 ) ) ;
#9911 = CARTESIAN_POINT ( 'NONE',  ( -19.99999999999999645, -9.000000000000003553, 5.000000000000079936 ) ) ;
#9912 = VERTEX_POINT ( 'NONE', #5189 ) ;
#9913 = DIRECTION ( 'NONE',  ( 0.000000000000000000, 0.000000000000000000, 1.000000000000000000 ) ) ;
#9914 = CARTESIAN_POINT ( 'NONE',  ( -1.656854249492380804, 4.000000000000000000, 5.237500002731186655 ) ) ;
#9915 = CARTESIAN_POINT ( 'NONE',  ( -69.55000000109247082, 11.46158073645647235, 16.46158073645647235 ) ) ;
#9916 = EDGE_LOOP ( 'NONE', ( #8820, #12731, #827, #16414, #14958, #22208 ) ) ;
#9917 = ORIENTED_EDGE ( 'NONE', *, *, #110, .F. ) ;
#9918 = AXIS2_PLACEMENT_3D ( 'NONE', #12727, #10917, #21418 ) ;
#9919 = CARTESIAN_POINT ( 'NONE',  ( -2.000000000000007550, -3.464101615137749945, 0.000000000000000000 ) ) ;
#9920 = AXIS2_PLACEMENT_3D ( 'NONE', #16272, #23682, #12704 ) ;
#9921 = CARTESIAN_POINT ( 'NONE',  ( 51.37500000000000711, 7.171572875253794166, 12.17157287525381726 ) ) ;
#9922 = ORIENTED_EDGE ( 'NONE', *, *, #19154, .F. ) ;
#9923 = DIRECTION ( 'NONE',  ( -1.000000000000000000, -0.000000000000000000, 0.000000000000000000 ) ) ;
#9924 = VECTOR ( 'NONE', #9365, 1000.000000000000000 ) ;
#9925 = CARTESIAN_POINT ( 'NONE',  ( 67.35000000109248219, 8.538419263543522320, 16.46158073645647235 ) ) ;
#9926 = AXIS2_PLACEMENT_3D ( 'NONE', #6113, #591, #9837 ) ;
#9927 = CARTESIAN_POINT ( 'NONE',  ( 69.35000000109246798, 8.538419263543524096, 13.53841926354352054 ) ) ;
#9928 = ORIENTED_EDGE ( 'NONE', *, *, #16511, .T. ) ;
#9929 = EDGE_CURVE ( 'NONE', #9912, #22668, #21789, .T. ) ;
#9930 = DIRECTION ( 'NONE',  ( -0.000000000000000000, -0.000000000000000000, -1.000000000000000000 ) ) ;
#9931 = CIRCLE ( 'NONE', #19473, 5.000000000000011546 ) ;
#9932 = CARTESIAN_POINT ( 'NONE',  ( 55.87500000000000711, 7.171572875253794166, 12.17157287525381726 ) ) ;
#9933 = CARTESIAN_POINT ( 'NONE',  ( -1.067197363239236862, -6.889406814520513400, -3.442664554191213977 ) ) ;
#9934 = CARTESIAN_POINT ( 'NONE',  ( 1.025207404391860050E-15, 3.458734125000000326, 18.18750000136560274 ) ) ;
#9935 = DIRECTION ( 'NONE',  ( 0.000000000000000000, 0.5877852522924684742, 0.8090169943749507819 ) ) ;
#9936 = LINE ( 'NONE', #10420, #16294 ) ;
#9937 = ORIENTED_EDGE ( 'NONE', *, *, #15476, .T. ) ;
#9938 = AXIS2_PLACEMENT_3D ( 'NONE', #22109, #12935, #18653 ) ;
#9939 = FACE_OUTER_BOUND ( 'NONE', #8149, .T. ) ;
#9940 = CARTESIAN_POINT ( 'NONE',  ( 3.999999999999999112, 1.505528603326912629, 1.981791683554507300 ) ) ;
#9941 = CARTESIAN_POINT ( 'NONE',  ( -70.89999999999999147, 9.999999999999998224, 17.49999999999999645 ) ) ;
#9942 = AXIS2_PLACEMENT_3D ( 'NONE', #18909, #11399, #18552 ) ;
#9943 = EDGE_CURVE ( 'NONE', #8315, #23413, #14434, .T. ) ;
#9944 = ORIENTED_EDGE ( 'NONE', *, *, #21343, .F. ) ;
#9945 = CIRCLE ( 'NONE', #3791, 4.000000000000000000 ) ;
#9946 = DIRECTION ( 'NONE',  ( 0.000000000000000000, -1.000000000000000000, 0.000000000000000000 ) ) ;
#9947 = CARTESIAN_POINT ( 'NONE',  ( 2.499999999999999556, -7.593217523260641144, 7.958834565716742304 ) ) ;
#9948 = DIRECTION ( 'NONE',  ( -1.000000000000000000, 0.000000000000000000, -0.000000000000000000 ) ) ;
#9949 = EDGE_LOOP ( 'NONE', ( #14034, #16004, #15692, #8920 ) ) ;
#9950 = DIRECTION ( 'NONE',  ( 0.000000000000000000, 0.000000000000000000, -1.000000000000000000 ) ) ;
#9951 = VERTEX_POINT ( 'NONE', #18592 ) ;
#9952 = CARTESIAN_POINT ( 'NONE',  ( -31.74999999999995737, 0.000000000000000000, 4.250000000000000000 ) ) ;
#9953 =( GEOMETRIC_REPRESENTATION_CONTEXT ( 3 ) GLOBAL_UNCERTAINTY_ASSIGNED_CONTEXT ( ( #8128 ) ) GLOBAL_UNIT_ASSIGNED_CONTEXT ( ( #8580, #17790, #16000 ) ) REPRESENTATION_CONTEXT ( 'NONE', 'WORKASPACE' ) );
#9954 = CARTESIAN_POINT ( 'NONE',  ( 71.30000000109249925, 9.143825827087049163, 17.06698730000000097 ) ) ;
#9955 = CARTESIAN_POINT ( 'NONE',  ( -3.999999999999998224, -1.656854249492383246, 12.06250000000001243 ) ) ;
#9956 = CARTESIAN_POINT ( 'NONE',  ( 71.05000000218495870, 8.964466094067258695, 17.50000000000000355 ) ) ;
#9957 = ORIENTED_EDGE ( 'NONE', *, *, #9637, .F. ) ;
#9958 = DIRECTION ( 'NONE',  ( 0.000000000000000000, 0.000000000000000000, 1.000000000000000000 ) ) ;
#9959 = DIRECTION ( 'NONE',  ( 1.000000000000000000, 0.000000000000000000, 0.000000000000000000 ) ) ;
#9960 = CARTESIAN_POINT ( 'NONE',  ( 67.05000000109247082, 9.999999999999998224, 12.93301269999999192 ) ) ;
#9961 = CIRCLE ( 'NONE', #16071, 11.00000000000000000 ) ;
#9962 = VERTEX_POINT ( 'NONE', #18473 ) ;
#9963 = EDGE_CURVE ( 'NONE', #13999, #2500, #14673, .T. ) ;
#9964 = CARTESIAN_POINT ( 'NONE',  ( 0.000000000000000000, 0.000000000000000000, 0.000000000000000000 ) ) ;
#9965 = ADVANCED_FACE ( 'NONE', ( #4099 ), #16930, .F. ) ;
#9966 = CARTESIAN_POINT ( 'NONE',  ( -3.999999999999999112, 0.000000000000000000, 21.31370849898476649 ) ) ;
#9967 = CARTESIAN_POINT ( 'NONE',  ( 69.05000000109247082, 9.999999999999998224, 17.06698730000000097 ) ) ;
#9968 = CARTESIAN_POINT ( 'NONE',  ( 1.025207404391860050E-15, 3.458734125000000326, 12.18750000136560629 ) ) ;
#9969 = AXIS2_PLACEMENT_3D ( 'NONE', #3776, #9207, #21739 ) ;
#9970 = LINE ( 'NONE', #17263, #2467 ) ;
#9971 = CYLINDRICAL_SURFACE ( 'NONE', #18399, 2.499999999999998668 ) ;
#9972 = ORIENTED_EDGE ( 'NONE', *, *, #12351, .T. ) ;
#9973 = CARTESIAN_POINT ( 'NONE',  ( -4.000000000000000000, 0.000000000000000000, 2.300000000000001599 ) ) ;
#9974 = CARTESIAN_POINT ( 'NONE',  ( -3.999999999999999112, 1.656854249492380582, 15.93750000000001066 ) ) ;
#9975 = DIRECTION ( 'NONE',  ( 0.000000000000000000, 0.000000000000000000, 1.000000000000000000 ) ) ;
#9976 = CARTESIAN_POINT ( 'NONE',  ( -2.762848947613219419, 4.746226468750993632, -19.99999999999999645 ) ) ;
#9977 = EDGE_CURVE ( 'NONE', #5706, #6890, #5542, .T. ) ;
#9978 = ADVANCED_FACE ( 'NONE', ( #11318 ), #11075, .T. ) ;
#9979 = ORIENTED_EDGE ( 'NONE', *, *, #8208, .F. ) ;
#9980 = CARTESIAN_POINT ( 'NONE',  ( -66.30000000109247082, 12.06698729999999919, 15.85617417291294196 ) ) ;
#9981 = EDGE_LOOP ( 'NONE', ( #10338, #21540, #20634, #2321 ) ) ;
#9982 = CARTESIAN_POINT ( 'NONE',  ( -66.50000000109245946, 12.06698730000000275, 15.85617417291294196 ) ) ;
#9983 = ITEM_DEFINED_TRANSFORMATION ( 'NONE', 'NONE', #21754,  #7318 ) ;
#9984 = VERTEX_POINT ( 'NONE', #6021 ) ;
#9985 = LINE ( 'NONE', #6133, #10949 ) ;
#9986 = EDGE_LOOP ( 'NONE', ( #20862, #2756, #7873, #3696 ) ) ;
#9987 = VECTOR ( 'NONE', #22226, 1000.000000000000000 ) ;
#9988 = VERTEX_POINT ( 'NONE', #15150 ) ;
#9989 = CARTESIAN_POINT ( 'NONE',  ( -3.458734124999999437, 1.432654583217640498, 13.62500000136560452 ) ) ;
#9990 = CARTESIAN_POINT ( 'NONE',  ( 45.00000000000000000, 15.00000000000003375, 34.11836509645780069 ) ) ;
#9991 = AXIS2_PLACEMENT_3D ( 'NONE', #4800, #14036, #17636 ) ;
#9992 = CARTESIAN_POINT ( 'NONE',  ( -66.90000000109246514, 10.85617417291294551, 12.93301269999999370 ) ) ;
#9993 = VECTOR ( 'NONE', #19385, 1000.000000000000114 ) ;
#9994 = EDGE_CURVE ( 'NONE', #22866, #15279, #17232, .T. ) ;
#9995 = CARTESIAN_POINT ( 'NONE',  ( 68.75000000109247367, 11.46158073645647235, 16.46158073645647235 ) ) ;
#9996 = CARTESIAN_POINT ( 'NONE',  ( -67.90000000109245093, 10.85617417291294551, 12.93301269999999370 ) ) ;
#9997 = EDGE_CURVE ( 'NONE', #12317, #15248, #4214, .T. ) ;
#9998 = CARTESIAN_POINT ( 'NONE',  ( 55.00000000000000711, -9.999999999999998224, 20.00000000000001421 ) ) ;
#9999 = CARTESIAN_POINT ( 'NONE',  ( 55.93518183416157541, 9.931948859054372747, 17.99999999999999645 ) ) ;
#10000 = FACE_OUTER_BOUND ( 'NONE', #1174, .T. ) ;
#10001 = CARTESIAN_POINT ( 'NONE',  ( -2.445694354108820523, 2.445694354108820523, 1.862500001365596347 ) ) ;
#10002 = CARTESIAN_POINT ( 'NONE',  ( -2.500000000000000888, 0.000000000000000000, -4.974599999999998801 ) ) ;
#10003 = CARTESIAN_POINT ( 'NONE',  ( -2.828427124746188515, -2.828427124746190735, 10.25000000273119660 ) ) ;
#10004 = CARTESIAN_POINT ( 'NONE',  ( 65.00000000000000000, -9.999999999999998224, 24.99999999999999645 ) ) ;
#10005 = ADVANCED_FACE ( 'NONE', ( #18361 ), #12995, .T. ) ;
#10006 = CIRCLE ( 'NONE', #4631, 4.000000000000001776 ) ;
#10007 = ADVANCED_FACE ( 'NONE', ( #18715 ), #2052, .F. ) ;
#10008 = ORIENTED_EDGE ( 'NONE', *, *, #5733, .T. ) ;
#10009 = CARTESIAN_POINT ( 'NONE',  ( 4.000000000000000888, 4.898587196589412829E-16, 13.50000000000001066 ) ) ;
#10010 = VERTEX_POINT ( 'NONE', #390 ) ;
#10011 = CARTESIAN_POINT ( 'NONE',  ( 60.06018183416157541, 7.000000000000000000, 14.93194885905437097 ) ) ;
#10012 = DIRECTION ( 'NONE',  ( 1.000000000000000000, 0.000000000000000000, 0.000000000000000000 ) ) ;
#10013 = CARTESIAN_POINT ( 'NONE',  ( 3.458734125000000326, 4.235727675282971730E-16, 0.2375000013655967357 ) ) ;
#10014 = CARTESIAN_POINT ( 'NONE',  ( -1.432654583217640942, -3.458734124999999882, 0.9250000013655965692 ) ) ;
#10015 = ORIENTED_EDGE ( 'NONE', *, *, #6402, .T. ) ;
#10016 = CARTESIAN_POINT ( 'NONE',  ( -90.00000000000000000, 0.000000000000000000, 0.000000000000000000 ) ) ;
#10017 =( NAMED_UNIT ( * ) PLANE_ANGLE_UNIT ( ) SI_UNIT ( $, .RADIAN. ) );
#10018 = ORIENTED_EDGE ( 'NONE', *, *, #12301, .F. ) ;
#10019 = CARTESIAN_POINT ( 'NONE',  ( -72.50000000000000000, 9.999999999999998224, 14.99999999999999645 ) ) ;
#10020 = VERTEX_POINT ( 'NONE', #20374 ) ;
#10021 = CARTESIAN_POINT ( 'NONE',  ( 56.65856816583844591, 7.028187705514647554, 16.31069182806492179 ) ) ;
#10022 = CARTESIAN_POINT ( 'NONE',  ( -69.25000000218494733, 12.50000000000000000, 16.03553390593273420 ) ) ;
#10023 = CARTESIAN_POINT ( 'NONE',  ( -3.458734125000000326, -1.432654583217642497, -2.949999998634404985 ) ) ;
#10024 = AXIS2_PLACEMENT_3D ( 'NONE', #15098, #18532, #3574 ) ;
#10025 = CARTESIAN_POINT ( 'NONE',  ( 1.656854249492384135, -3.999999999999999112, 15.31250000000001243 ) ) ;
#10026 =( BOUNDED_CURVE ( )  B_SPLINE_CURVE ( 2, ( #12021, #6727, #8649, #23231, #6499, #2995, #14037, #10586, #12135 ),
 .UNSPECIFIED., .F., .F. ) 
 B_SPLINE_CURVE_WITH_KNOTS ( ( 3, 2, 2, 2, 3 ),
 ( 0.7499999999999997780, 0.7656249999999996669, 0.7812499999999995559, 0.7968749999999994449, 0.8124999999999993339 ),
 .UNSPECIFIED. ) 
 CURVE ( )  GEOMETRIC_REPRESENTATION_ITEM ( )  RATIONAL_B_SPLINE_CURVE ( ( 1.000000000000001110, 0.9238795325112856283, 1.000000000000000000, 0.9238795325112867385, 1.000000000000000000, 0.9238795325112867385, 1.000000000000000000, 0.9238795325112899581, 0.9999999999999967804 ) ) 
 REPRESENTATION_ITEM ( '' )  );
#10027 = CARTESIAN_POINT ( 'NONE',  ( -2.445694354108818303, -2.445694354108820967, 17.81250000136560274 ) ) ;
#10028 = DIRECTION ( 'NONE',  ( 1.000000000000000000, 7.703719777548943412E-32, 0.000000000000000000 ) ) ;
#10029 = CARTESIAN_POINT ( 'NONE',  ( 70.00000000109248788, 9.143825827087050939, 12.93301269999999370 ) ) ;
#10030 = LINE ( 'NONE', #19213, #15711 ) ;
#10031 = CARTESIAN_POINT ( 'NONE',  ( 53.00231816583844591, 12.07320092032949610, 12.83056023321021044 ) ) ;
#10032 = CARTESIAN_POINT ( 'NONE',  ( 1.432654583217642275, -3.458734124999999882, 5.300000001365596347 ) ) ;
#10033 = DIRECTION ( 'NONE',  ( -1.000000000000000000, -0.000000000000000000, -0.000000000000000000 ) ) ;
#10034 = ADVANCED_FACE ( 'NONE', ( #20618 ), #258, .F. ) ;
#10035 = DIRECTION ( 'NONE',  ( -1.000000000000000000, 0.000000000000000000, 1.224646799147353454E-16 ) ) ;
#10036 = CARTESIAN_POINT ( 'NONE',  ( -69.55000000109247082, 11.46158073645647235, 13.53841926354352232 ) ) ;
#10037 = ADVANCED_FACE ( 'NONE', ( #4225 ), #11561, .F. ) ;
#10038 = CARTESIAN_POINT ( 'NONE',  ( -69.80000000218494449, 9.999999999999998224, 12.49999999999999289 ) ) ;
#10039 = CARTESIAN_POINT ( 'NONE',  ( -35.00000000000000000, 7.500000000000001776, -19.99999999999998934 ) ) ;
#10040 = ORIENTED_EDGE ( 'NONE', *, *, #15851, .F. ) ;
#10041 = DIRECTION ( 'NONE',  ( 0.000000000000000000, 0.000000000000000000, 1.000000000000000000 ) ) ;
#10042 = CARTESIAN_POINT ( 'NONE',  ( 72.50000000000000000, 9.999999999999998224, 14.99999999999999645 ) ) ;
#10043 = EDGE_LOOP ( 'NONE', ( #11752, #16765, #4191, #1135 ) ) ;
#10044 = ORIENTED_EDGE ( 'NONE', *, *, #15412, .F. ) ;
#10045 = FACE_OUTER_BOUND ( 'NONE', #22641, .T. ) ;
#10046 = CARTESIAN_POINT ( 'NONE',  ( 53.06250000000000711, 5.999999999999996447, 15.00000000000001599 ) ) ;
#10047 = VERTEX_POINT ( 'NONE', #16456 ) ;
#10048 = CARTESIAN_POINT ( 'NONE',  ( -0.1404048886732797152, -4.699864953788083888, -3.686887068327043160 ) ) ;
#10049 = PRODUCT_DEFINITION_CONTEXT ( 'detailed design', #3943, 'design' ) ;
#10050 = CARTESIAN_POINT ( 'NONE',  ( 67.80000000109247082, 12.06698730000000275, 14.14382582708705094 ) ) ;
#10051 = CARTESIAN_POINT ( 'NONE',  ( 69.60000000109248219, 12.06698730000000275, 14.14382582708705094 ) ) ;
#10052 = ORIENTED_EDGE ( 'NONE', *, *, #22460, .F. ) ;
#10053 = CARTESIAN_POINT ( 'NONE',  ( 118.3095189484530181, -14.69846310392956745, 35.82846581308617573 ) ) ;
#10054 = CARTESIAN_POINT ( 'NONE',  ( 58.12500000000000000, 12.82842712474620228, 17.82842712474617386 ) ) ;
#10055 = LINE ( 'NONE', #19238, #9251 ) ;
#10056 = CARTESIAN_POINT ( 'NONE',  ( -3.458734124999998993, 0.000000000000000000, 19.43750000136560629 ) ) ;
#10057 = CARTESIAN_POINT ( 'NONE',  ( 65.00000000000000000, 15.00000000000000000, 10.00000000000007105 ) ) ;
#10058 = CARTESIAN_POINT ( 'NONE',  ( 50.00000000000002132, -10.03966385473554013, 5.000000000000079936 ) ) ;
#10059 = ORIENTED_EDGE ( 'NONE', *, *, #12888, .T. ) ;
#10060 = LINE ( 'NONE', #17350, #383 ) ;
#10061 = CARTESIAN_POINT ( 'NONE',  ( 0.000000000000000000, 10.82112760146739383, -1.975651141462125171 ) ) ;
#10062 = DIRECTION ( 'NONE',  ( 0.000000000000000000, 0.000000000000000000, -1.000000000000000000 ) ) ;
#10063 = ORIENTED_EDGE ( 'NONE', *, *, #12379, .T. ) ;
#10064 = CARTESIAN_POINT ( 'NONE',  ( 6.405354440716562792, -8.974600000000002353, 10.00000000000008882 ) ) ;
#10065 = CARTESIAN_POINT ( 'NONE',  ( 36.10423233033275636, -11.25000000000000355, 5.000000000000079936 ) ) ;
#10066 = CARTESIAN_POINT ( 'NONE',  ( -18.12177574676618974, -9.000000000000003553, 10.00000000000008882 ) ) ;
#10067 = PRODUCT_RELATED_PRODUCT_CATEGORY ( 'part', '', ( #11660 ) ) ;
#10068 = VECTOR ( 'NONE', #21383, 1000.000000000000114 ) ;
#10069 = CARTESIAN_POINT ( 'NONE',  ( 4.999999999999999112, 4.472189673936787457, 8.264486777890123648 ) ) ;
#10070 = VERTEX_POINT ( 'NONE', #20129 ) ;
#10071 = CARTESIAN_POINT ( 'NONE',  ( 5.434916218090827478, 4.367703157927330437, -3.442152416367929568 ) ) ;
#10073 = VERTEX_POINT ( 'NONE', #1942 ) ;
#10072 = AXIS2_PLACEMENT_3D ( 'NONE', #1091, #6622, #21198 ) ;
#10074 = EDGE_CURVE ( 'NONE', #10654, #17879, #17619, .T. ) ;
#10075 = DIRECTION ( 'NONE',  ( 0.9396926207859107594, -0.3420201433256623291, 3.697785493223492838E-32 ) ) ;
#10076 = DIRECTION ( 'NONE',  ( 0.000000000000000000, -6.938893903907226800E-15, 1.000000000000000000 ) ) ;
#10077 = LINE ( 'NONE', #6584, #1114 ) ;
#10078 = CARTESIAN_POINT ( 'NONE',  ( 45.00000000000000000, 10.00000000000001599, 15.00000000000003020 ) ) ;
#10079 = CARTESIAN_POINT ( 'NONE',  ( 68.95000000109247651, 11.46158073645647235, 16.46158073645647235 ) ) ;
#10080 = ORIENTED_EDGE ( 'NONE', *, *, #5101, .F. ) ;
#10081 = FACE_BOUND ( 'NONE', #17705, .T. ) ;
#10082 = DIRECTION ( 'NONE',  ( 0.000000000000000000, -1.000000000000000000, 0.000000000000000000 ) ) ;
#10083 = CARTESIAN_POINT ( 'NONE',  ( 70.50000000109245946, 12.06698730000000275, 15.85617417291294196 ) ) ;
#10084 = CARTESIAN_POINT ( 'NONE',  ( 2.445694354108821411, 2.445694354108820523, 14.06250000136560452 ) ) ;
#10085 = LINE ( 'NONE', #22631, #20427 ) ;
#10086 = CARTESIAN_POINT ( 'NONE',  ( 4.999999999999999112, 4.729683950898872169, 7.360373001730934561 ) ) ;
#10087 = ORIENTED_EDGE ( 'NONE', *, *, #7938, .F. ) ;
#10088 = CARTESIAN_POINT ( 'NONE',  ( -4.000000000000000000, -1.656854249492383246, -0.6374999999999969580 ) ) ;
#10089 = CARTESIAN_POINT ( 'NONE',  ( 60.00000000000000711, 15.00000000000000000, 10.00000000000007105 ) ) ;
#10090 = CARTESIAN_POINT ( 'NONE',  ( -1.432654583217639610, -3.458734124999999882, 10.62500000136560274 ) ) ;
#10091 = CARTESIAN_POINT ( 'NONE',  ( -90.00000000000000000, 0.000000000000000000, 0.000000000000000000 ) ) ;
#10092 = VERTEX_POINT ( 'NONE', #22172 ) ;
#10093 = CARTESIAN_POINT ( 'NONE',  ( -67.05000000109247082, 12.06698730000000097, 14.99999999999999645 ) ) ;
#10094 = VERTEX_POINT ( 'NONE', #14794 ) ;
#10095 = CARTESIAN_POINT ( 'NONE',  ( -66.90000000109246514, 7.933012699999995476, 14.14382582708705094 ) ) ;
#10096 = ORIENTED_EDGE ( 'NONE', *, *, #7628, .T. ) ;
#10097 = DIRECTION ( 'NONE',  ( -1.000000000000000000, -7.703719777548943412E-32, 0.000000000000000000 ) ) ;
#10098 = ORIENTED_EDGE ( 'NONE', *, *, #17341, .T. ) ;
#10099 =( REPRESENTATION_RELATIONSHIP ('NONE','NONE', #8403, #21657 ) REPRESENTATION_RELATIONSHIP_WITH_TRANSFORMATION ( #6247 )SHAPE_REPRESENTATION_RELATIONSHIP( ) );
#10100 = EDGE_CURVE ( 'NONE', #19003, #5128, #1137, .T. ) ;
#10101 = EDGE_CURVE ( 'NONE', #25, #4980, #7592, .T. ) ;
#10102 = ORIENTED_EDGE ( 'NONE', *, *, #19023, .F. ) ;
#10103 = CARTESIAN_POINT ( 'NONE',  ( -3.458734124999998993, -1.432654583217642497, 12.75000000136560629 ) ) ;
#10104 = CARTESIAN_POINT ( 'NONE',  ( -2.828427124746190291, 2.828427124746190291, -0.6999999972688124572 ) ) ;
#10105 = VECTOR ( 'NONE', #19973, 1000.000000000000000 ) ;
#10106 = AXIS2_PLACEMENT_3D ( 'NONE', #12943, #18194, #5384 ) ;
#10107 = CARTESIAN_POINT ( 'NONE',  ( -19.99999999999999645, -9.000000000000003553, 5.000000000000079936 ) ) ;
#10108 = EDGE_CURVE ( 'NONE', #19663, #10566, #461, .T. ) ;
#10109 = CARTESIAN_POINT ( 'NONE',  ( -70.29999999999999716, 7.499999999999996447, 14.99999999999999645 ) ) ;
#10110 = LINE ( 'NONE', #8300, #6513 ) ;
#10111 = CARTESIAN_POINT ( 'NONE',  ( 60.90393183416158962, 14.02818770551463956, 13.41119689145323335 ) ) ;
#10112 = CARTESIAN_POINT ( 'NONE',  ( 59.99999999999999289, 12.81859298856320528, 13.90091681563048631 ) ) ;
#10113 = CARTESIAN_POINT ( 'NONE',  ( 3.458734125000000770, 4.235727675282972223E-16, 3.487500001365597679 ) ) ;
#10114 = DIRECTION ( 'NONE',  ( 0.000000000000000000, 1.224646799147367998E-16, 1.000000000000000000 ) ) ;
#10115 = CARTESIAN_POINT ( 'NONE',  ( -1.656854249492380138, -3.999999999999999112, 13.31250000273119660 ) ) ;
#10116 = CARTESIAN_POINT ( 'NONE',  ( 4.999999999999999112, 9.314797388894893615, 1.239665997526919083 ) ) ;
#10117 = ORIENTED_EDGE ( 'NONE', *, *, #1504, .F. ) ;
#10118 = FACE_BOUND ( 'NONE', #13462, .T. ) ;
#10119 = ORIENTED_EDGE ( 'NONE', *, *, #1015, .F. ) ;
#10120 = CARTESIAN_POINT ( 'NONE',  ( 58.84143183416158962, 8.275094609562001935, 18.97181229448536044 ) ) ;
#10121 = CARTESIAN_POINT ( 'NONE',  ( 0.000000000000000000, 0.000000000000000000, 0.000000000000000000 ) ) ;
#10122 = CARTESIAN_POINT ( 'NONE',  ( -3.458734125000000326, 1.432654583217640276, 0.6750000013655963471 ) ) ;
#10123 = EDGE_CURVE ( 'NONE', #14446, #12965, #4454, .T. ) ;
#10124 = CARTESIAN_POINT ( 'NONE',  ( -1.432654583217640276, 3.458734125000000326, -0.4499999986344046521 ) ) ;
#10125 = VERTEX_POINT ( 'NONE', #11916 ) ;
#10126 = CARTESIAN_POINT ( 'NONE',  ( 72.50000000000000000, 9.999999999999998224, 14.99999999999999645 ) ) ;
#10127 =( LENGTH_UNIT ( ) NAMED_UNIT ( * ) SI_UNIT ( .MILLI., .METRE. ) );
#10128 = EDGE_CURVE ( 'NONE', #22239, #4233, #1909, .T. ) ;
#10129 = VERTEX_POINT ( 'NONE', #4337 ) ;
#10130 = LINE ( 'NONE', #11938, #23655 ) ;
#10131 = EDGE_LOOP ( 'NONE', ( #15604, #11963, #20010, #17928 ) ) ;
#10132 = PRODUCT_DEFINITION_SHAPE ( 'NONE', 'NONE',  #23705 ) ;
#10133 = CARTESIAN_POINT ( 'NONE',  ( 58.62731816583843170, 12.16943976678978601, 17.07320092032949432 ) ) ;
#10134 = CARTESIAN_POINT ( 'NONE',  ( -68.85000000218495586, 7.499999999999995559, 13.96446609406725692 ) ) ;
#10135 = EDGE_CURVE ( 'NONE', #1904, #15027, #21295, .T. ) ;
#10136 = CARTESIAN_POINT ( 'NONE',  ( -1.432654583217640498, 3.458734125000000770, -3.199999998634403209 ) ) ;
#10137 = EDGE_CURVE ( 'NONE', #1712, #5354, #7291, .T. ) ;
#10138 = CARTESIAN_POINT ( 'NONE',  ( 1.236993788156008760E-15, 0.000000000000000000, 21.31370849898476649 ) ) ;
#10139 = CARTESIAN_POINT ( 'NONE',  ( -3.458734124999999437, 0.000000000000000000, 19.68750000136560629 ) ) ;
#10140 = CARTESIAN_POINT ( 'NONE',  ( 1.656854249492381470, 4.000000000000000000, 11.81250000273119838 ) ) ;
#10141 = VECTOR ( 'NONE', #8084, 1000.000000000000000 ) ;
#10142 = LINE ( 'NONE', #20758, #15843 ) ;
#10143 = CARTESIAN_POINT ( 'NONE',  ( 69.00000000109247367, 7.933012699999995476, 15.85617417291294196 ) ) ;
#10144 = CYLINDRICAL_SURFACE ( 'NONE', #11104, 2.500000000000002220 ) ;
#10145 = CARTESIAN_POINT ( 'NONE',  ( 54.68981816583844591, 9.931948859054354983, 11.99999999999999645 ) ) ;
#10146 = CARTESIAN_POINT ( 'NONE',  ( 1.432654583217642275, -3.458734124999999882, 1.300000001365597235 ) ) ;
#10147 = CARTESIAN_POINT ( 'NONE',  ( -10.00000000000000000, 0.000000000000000000, 0.000000000000000000 ) ) ;
#10148 = LINE ( 'NONE', #19102, #9199 ) ;
#10149 = CARTESIAN_POINT ( 'NONE',  ( -67.65000000109247935, 7.933012699999995476, 14.99999999999999645 ) ) ;
#10150 = FACE_OUTER_BOUND ( 'NONE', #8477, .T. ) ;
#10151 = CARTESIAN_POINT ( 'NONE',  ( 0.000000000000000000, -8.152713396088739017, -3.174628368996162298 ) ) ;
#10152 = EDGE_LOOP ( 'NONE', ( #10864, #10833, #5291, #8178 ) ) ;
#10153 = CARTESIAN_POINT ( 'NONE',  ( 1.971781867644420635E-15, -4.000000000000000000, 14.25000000000001066 ) ) ;
#10154 = AXIS2_PLACEMENT_3D ( 'NONE', #22873, #2401, #953 ) ;
#10155 = SURFACE_SIDE_STYLE ('',( #1242 ) ) ;
#10156 = CARTESIAN_POINT ( 'NONE',  ( 4.000000000000000000, 1.656854249492381248, 2.987500002731188431 ) ) ;
#10157 = AXIS2_PLACEMENT_3D ( 'NONE', #6820, #1182, #10326 ) ;
#10158 = VERTEX_POINT ( 'NONE', #4693 ) ;
#10159 = ORIENTED_EDGE ( 'NONE', *, *, #11605, .T. ) ;
#10160 = DIRECTION ( 'NONE',  ( -1.000000000000000000, 0.000000000000000000, 0.000000000000000000 ) ) ;
#10161 = CARTESIAN_POINT ( 'NONE',  ( -66.84999999999999432, 11.03553390593268624, 17.50000000000005329 ) ) ;
#10162 = ORIENTED_EDGE ( 'NONE', *, *, #19308, .T. ) ;
#10163 = DIRECTION ( 'NONE',  ( -1.224646799147353207E-16, 0.000000000000000000, -1.000000000000000000 ) ) ;
#10164 = EDGE_CURVE ( 'NONE', #25, #10781, #1085, .T. ) ;
#10165 = EDGE_CURVE ( 'NONE', #6714, #15383, #10110, .T. ) ;
#10166 = CARTESIAN_POINT ( 'NONE',  ( 67.55000000109247082, 8.538419263543524096, 13.53841926354352054 ) ) ;
#10167 = VECTOR ( 'NONE', #5502, 1000.000000000000000 ) ;
#10168 = ADVANCED_FACE ( 'NONE', ( #15621 ), #744, .F. ) ;
#10169 = CIRCLE ( 'NONE', #10931, 0.2000000000000000944 ) ;
#10170 = CARTESIAN_POINT ( 'NONE',  ( 68.35000000109246798, 8.538419263543522320, 16.46158073645647235 ) ) ;
#10171 = AXIS2_PLACEMENT_3D ( 'NONE', #10990, #3545, #10881 ) ;
#10172 = ORIENTED_EDGE ( 'NONE', *, *, #14552, .T. ) ;
#10173 = CARTESIAN_POINT ( 'NONE',  ( 27.56832511966726784, -11.25000000000000355, 10.00000000000008882 ) ) ;
#10174 = CARTESIAN_POINT ( 'NONE',  ( 55.40625000000000000, 13.99999999999999289, 13.34314575050759544 ) ) ;
#10175 = DIRECTION ( 'NONE',  ( 0.000000000000000000, 0.000000000000000000, -1.000000000000000000 ) ) ;
#10176 = CARTESIAN_POINT ( 'NONE',  ( -2.445694354108819191, 2.445694354108820523, 17.31250000136560274 ) ) ;
#10177 = CYLINDRICAL_SURFACE ( 'NONE', #19698, 2.500000000000002220 ) ;
#10178 = DIRECTION ( 'NONE',  ( -1.000000000000000000, -0.000000000000000000, -0.000000000000000000 ) ) ;
#10179 = EDGE_LOOP ( 'NONE', ( #20572, #9554, #5897, #5862 ) ) ;
#10180 = FACE_BOUND ( 'NONE', #18775, .T. ) ;
#10181 = DIRECTION ( 'NONE',  ( 0.9396926207859107594, -0.3420201433256623291, 3.697785493223492838E-32 ) ) ;
#10182 = LINE ( 'NONE', #23436, #3908 ) ;
#10183 = VERTEX_POINT ( 'NONE', #19291 ) ;
#10184 = DIRECTION ( 'NONE',  ( 1.000000000000000000, -0.000000000000000000, -0.000000000000000000 ) ) ;
#10185 = CARTESIAN_POINT ( 'NONE',  ( -4.000000000000000000, -2.309401076758512694, -5.000000000000000000 ) ) ;
#10186 = CIRCLE ( 'NONE', #9036, 2.500000000000007550 ) ;
#10187 = CIRCLE ( 'NONE', #23153, 9.999999999999996447 ) ;
#10188 = CARTESIAN_POINT ( 'NONE',  ( -70.80000000218494449, 12.50000000000000000, 14.99999999999999645 ) ) ;
#10189 = ORIENTED_EDGE ( 'NONE', *, *, #8484, .F. ) ;
#10190 = CARTESIAN_POINT ( 'NONE',  ( -69.70000000000000284, 9.999999999999998224, 12.49999999999999289 ) ) ;
#10191 = ORIENTED_EDGE ( 'NONE', *, *, #23395, .T. ) ;
#10192 = LINE ( 'NONE', #8152, #14491 ) ;
#10193 = CARTESIAN_POINT ( 'NONE',  ( 70.40000000218495302, 7.499999999999996447, 14.99999999999999645 ) ) ;
#10194 = CIRCLE ( 'NONE', #11342, 0.1999999999999996503 ) ;
#10195 = AXIS2_PLACEMENT_3D ( 'NONE', #18925, #8054, #17267 ) ;
#10196 = CARTESIAN_POINT ( 'NONE',  ( -17.30284271966725029, -11.25000000000000355, 5.000000000000079936 ) ) ;
#10197 = CARTESIAN_POINT ( 'NONE',  ( -3.333333333333332149, -2.694301256218264218, -3.300726591567082036 ) ) ;
#10198 = CARTESIAN_POINT ( 'NONE',  ( 67.50000000109245946, 9.143825827087049163, 17.06698730000000097 ) ) ;
#10199 = ORIENTED_EDGE ( 'NONE', *, *, #12946, .F. ) ;
#10200 = VECTOR ( 'NONE', #19394, 1000.000000000000000 ) ;
#10201 = CARTESIAN_POINT ( 'NONE',  ( -68.70000000218495018, 8.232233047033627571, 16.76776695296636532 ) ) ;
#10202 = CARTESIAN_POINT ( 'NONE',  ( -3.999999999999999112, 0.000000000000000000, 10.12500000273119660 ) ) ;
#10203 = CARTESIAN_POINT ( 'NONE',  ( 68.40000000109246514, 7.933012699999995476, 15.85617417291294196 ) ) ;
#10204 = CARTESIAN_POINT ( 'NONE',  ( -1.432654583217639832, -3.458734125000000326, 18.87500000136560274 ) ) ;
#10205 = CYLINDRICAL_SURFACE ( 'NONE', #1316, 2.500000000000002220 ) ;
#10206 = EDGE_CURVE ( 'NONE', #10458, #12128, #22946, .T. ) ;
#10207 = DIRECTION ( 'NONE',  ( 0.000000000000000000, 0.000000000000000000, 1.000000000000000000 ) ) ;
#10208 = ORIENTED_EDGE ( 'NONE', *, *, #17979, .T. ) ;
#10209 = CARTESIAN_POINT ( 'NONE',  ( 7.347880794884118750E-16, -4.000000000000000000, -2.449999999999998845 ) ) ;
#10210 = DIRECTION ( 'NONE',  ( 0.000000000000000000, -1.000000000000000000, -0.000000000000000000 ) ) ;
#10211 = CARTESIAN_POINT ( 'NONE',  ( -10.00000000000000000, 0.000000000000000000, 0.000000000000000000 ) ) ;
#10212 = DIRECTION ( 'NONE',  ( 1.000000000000000000, 0.000000000000000000, 0.000000000000000000 ) ) ;
#10213 = ORIENTED_EDGE ( 'NONE', *, *, #585, .F. ) ;
#10214 = DIRECTION ( 'NONE',  ( 0.000000000000000000, 0.000000000000000000, 1.000000000000000000 ) ) ;
#10215 = ORIENTED_EDGE ( 'NONE', *, *, #22325, .F. ) ;
#10216 = CARTESIAN_POINT ( 'NONE',  ( -68.85000000109246798, 12.06698730000000097, 14.99999999999999645 ) ) ;
#10217 = ORIENTED_EDGE ( 'NONE', *, *, #904, .T. ) ;
#10218 = CARTESIAN_POINT ( 'NONE',  ( -8.696997796766190447, -9.000000000000005329, 5.000000000000079936 ) ) ;
#10219 = EDGE_LOOP ( 'NONE', ( #19269, #22939, #693, #17759 ) ) ;
#10220 = EDGE_LOOP ( 'NONE', ( #1840, #11555, #9566, #22515 ) ) ;
#10221 = CARTESIAN_POINT ( 'NONE',  ( -3.458734124999999437, 0.000000000000000000, 13.68750000136560629 ) ) ;
#10222 = CARTESIAN_POINT ( 'NONE',  ( 1.656854249492380138, 4.000000000000000000, -0.8874999972688127903 ) ) ;
#10223 = CARTESIAN_POINT ( 'NONE',  ( -90.00000000000000000, 0.000000000000000000, 0.000000000000000000 ) ) ;
#10224 = CARTESIAN_POINT ( 'NONE',  ( 67.30000000109247082, 9.143825827087049163, 17.06698730000000097 ) ) ;
#10225 = CARTESIAN_POINT ( 'NONE',  ( -71.00000000000000000, 8.232233047033627571, 16.76776695296636532 ) ) ;
#10226 = SHAPE_REPRESENTATION ( 'End Stop Bumper spring', ( #7318 ), #9953 ) ;
#10227 = CARTESIAN_POINT ( 'NONE',  ( 6.500000000000000000, -3.142418015001833265, -0.4043611937012248636 ) ) ;
#10228 = CARTESIAN_POINT ( 'NONE',  ( 52.27893183416158251, 8.825410453826341595, 11.97181229448535511 ) ) ;
#10229 = DIRECTION ( 'NONE',  ( 0.000000000000000000, -0.5000000000000013323, -0.8660254037844380415 ) ) ;
#10230 = ADVANCED_FACE ( 'NONE', ( #22538 ), #19064, .T. ) ;
#10231 = CIRCLE ( 'NONE', #2548, 6.500000000000000888 ) ;
#10232 = CARTESIAN_POINT ( 'NONE',  ( -3.458734125000000770, 1.432654583217640498, -1.074999998634403209 ) ) ;
#10233 = CARTESIAN_POINT ( 'NONE',  ( 2.500000000000000000, 1.768423874527822459, -1.021000000000002794 ) ) ;
#10234 = CARTESIAN_POINT ( 'NONE',  ( -14.99999999999996980, 15.00000000000000000, -19.99999999999999645 ) ) ;
#10235 = CARTESIAN_POINT ( 'NONE',  ( 9.920644283265380691E-16, 4.000000000000000000, 12.87500000273119660 ) ) ;
#10236 = DIRECTION ( 'NONE',  ( -0.000000000000000000, -1.000000000000000000, -0.000000000000000000 ) ) ;
#10237 = APPLICATION_CONTEXT ( 'automotive_design' ) ;
#10238 = ORIENTED_EDGE ( 'NONE', *, *, #17133, .T. ) ;
#10239 = CARTESIAN_POINT ( 'NONE',  ( -3.999999999999999112, 1.656854249492380582, 13.93750000000001243 ) ) ;
#10240 = ORIENTED_EDGE ( 'NONE', *, *, #15677, .T. ) ;
#10241 = CARTESIAN_POINT ( 'NONE',  ( 53.77893183416158251, 8.825410453826341595, 11.97181229448535511 ) ) ;
#10242 = EDGE_CURVE ( 'NONE', #3630, #15866, #15333, .T. ) ;
#10243 = CARTESIAN_POINT ( 'NONE',  ( -1.432654583217640276, 3.458734125000000326, 0.5500000013655963471 ) ) ;
#10244 = VERTEX_POINT ( 'NONE', #2530 ) ;
#10245 = CIRCLE ( 'NONE', #23601, 11.00000000000000000 ) ;
#10246 = DIRECTION ( 'NONE',  ( -1.000000000000000000, -0.000000000000000000, -0.000000000000000000 ) ) ;
#10247 = ORIENTED_EDGE ( 'NONE', *, *, #15382, .T. ) ;
#10248 = CARTESIAN_POINT ( 'NONE',  ( 4.000000000000000888, 1.656854249492381248, 19.56250000000001421 ) ) ;
#10249 = VERTEX_POINT ( 'NONE', #9869 ) ;
#10250 = CARTESIAN_POINT ( 'NONE',  ( 55.90856816583843880, 12.97181229448534978, 13.68930817193506755 ) ) ;
#10251 = CARTESIAN_POINT ( 'NONE',  ( -66.55000000218494449, 8.964466094067258695, 12.49999999999999289 ) ) ;
#10252 = CARTESIAN_POINT ( 'NONE',  ( 2.500000000000000000, 1.768423874527823791, 1.020999999999998353 ) ) ;
#10253 = AXIS2_PLACEMENT_3D ( 'NONE', #1499, #16246, #19936 ) ;
#10254 = CARTESIAN_POINT ( 'NONE',  ( -3.847601380332740018, -11.25000000000000355, 5.000000000000079936 ) ) ;
#10255 = CARTESIAN_POINT ( 'NONE',  ( 3.458734125000001658, 4.235727675282972223E-16, 18.18750000136560274 ) ) ;
#10256 = CARTESIAN_POINT ( 'NONE',  ( -2.828427124746189403, 2.828427124746190291, 15.00000000273119660 ) ) ;
#10257 = CARTESIAN_POINT ( 'NONE',  ( 4.999999999999999112, 0.000000000000000000, 0.000000000000000000 ) ) ;
#10258 = AXIS2_PLACEMENT_3D ( 'NONE', #22698, #10160, #13398 ) ;
#10259 = CARTESIAN_POINT ( 'NONE',  ( 68.65000000109247935, 12.06698730000000097, 14.99999999999999645 ) ) ;
#10260 = CIRCLE ( 'NONE', #13316, 6.543750000000021494 ) ;
#10261 = ADVANCED_FACE ( 'NONE', ( #17164 ), #22653, .F. ) ;
#10262 = CARTESIAN_POINT ( 'NONE',  ( -4.198928548860774157, 0.8158838809860065044, -3.526471437616918170 ) ) ;
#10263 = CARTESIAN_POINT ( 'NONE',  ( 58.50000000000000000, 12.12132034355963484, 12.87867965644034740 ) ) ;
#10264 = ADVANCED_FACE ( 'NONE', ( #6260 ), #13580, .T. ) ;
#10265 = CARTESIAN_POINT ( 'NONE',  ( -2.117863837641485618E-16, 3.458734125000000770, 2.737500001365597235 ) ) ;
#10266 = DIRECTION ( 'NONE',  ( -1.000000000000000000, 0.000000000000000000, -0.000000000000000000 ) ) ;
#10267 = CARTESIAN_POINT ( 'NONE',  ( 25.86052135323381407, -9.000000000000003553, 5.000000000000079936 ) ) ;
#10268 = CARTESIAN_POINT ( 'NONE',  ( -69.70000000109247651, 12.06698729999999919, 15.85617417291294196 ) ) ;
#10269 = ORIENTED_EDGE ( 'NONE', *, *, #7446, .F. ) ;
#10270 = CARTESIAN_POINT ( 'NONE',  ( 0.1129242967662022479, -9.000000000000003553, 5.000000000000079936 ) ) ;
#10271 = CARTESIAN_POINT ( 'NONE',  ( 2.828427124746189847, 2.828427124746190291, -2.074999999999998845 ) ) ;
#10272 = ORIENTED_EDGE ( 'NONE', *, *, #17715, .F. ) ;
#10273 = CARTESIAN_POINT ( 'NONE',  ( 60.00000000000000711, 12.12132034355963484, 12.87867965644034740 ) ) ;
#10274 = CARTESIAN_POINT ( 'NONE',  ( 2.828427124746190735, -2.828427124746189847, 0.8000000027311872097 ) ) ;
#10275 = EDGE_CURVE ( 'NONE', #21235, #14801, #6380, .T. ) ;
#10276 = ORIENTED_EDGE ( 'NONE', *, *, #23598, .F. ) ;
#10277 = EDGE_CURVE ( 'NONE', #1550, #15217, #12504, .T. ) ;
#10278 = ORIENTED_EDGE ( 'NONE', *, *, #19457, .T. ) ;
#10279 = AXIS2_PLACEMENT_3D ( 'NONE', #3353, #8643, #23473 ) ;
#10280 = FACE_OUTER_BOUND ( 'NONE', #12954, .T. ) ;
#10281 = CARTESIAN_POINT ( 'NONE',  ( 0.000000000000000000, 1.699438267350500409, -9.241976615262139205 ) ) ;
#10282 = ORIENTED_EDGE ( 'NONE', *, *, #3538, .F. ) ;
#10283 = CARTESIAN_POINT ( 'NONE',  ( -65.00000000000000000, -10.00000000000000178, 12.49999999999999467 ) ) ;
#10284 = CIRCLE ( 'NONE', #1822, 0.03079999999999923077 ) ;
#10285 = PRESENTATION_LAYER_ASSIGNMENT (  '', '', ( #9898 ) ) ;
#10286 = CARTESIAN_POINT ( 'NONE',  ( 69.40000000109249356, 12.06698730000000275, 14.14382582708705094 ) ) ;
#10287 = CARTESIAN_POINT ( 'NONE',  ( 69.45000000109247651, 9.999999999999998224, 12.93301269999999192 ) ) ;
#10288 = LINE ( 'NONE', #8961, #3187 ) ;
#10289 = VECTOR ( 'NONE', #13191, 999.9999999999998863 ) ;
#10290 = DIRECTION ( 'NONE',  ( -1.000000000000000000, 0.000000000000000000, 0.000000000000000000 ) ) ;
#10291 = CARTESIAN_POINT ( 'NONE',  ( 53.62500000000000711, 12.82842712474620228, 17.82842712474617386 ) ) ;
#10292 = EDGE_CURVE ( 'NONE', #18952, #14717, #14289, .T. ) ;
#10293 = B_SPLINE_CURVE_WITH_KNOTS ( 'NONE', 3,
 ( #22925, #21109, #10262, #4725, #16195, #17318 ),
 .UNSPECIFIED., .F., .F.,
 ( 4, 2, 4 ),
 ( 0.002452478801916376308, 0.003676905084148007850, 0.004901331366379639391 ),
 .UNSPECIFIED. ) ;
#10294 = CARTESIAN_POINT ( 'NONE',  ( 2.445694354108820523, -2.445694354108820079, 3.112500001365597679 ) ) ;
#10295 = CARTESIAN_POINT ( 'NONE',  ( 3.458734125000001214, 1.432654583217640498, 13.00000000136560452 ) ) ;
#10296 = DIRECTION ( 'NONE',  ( -7.087422195345011518E-32, -1.000000000000000000, -0.000000000000000000 ) ) ;
#10297 = VECTOR ( 'NONE', #3022, 1000.000000000000000 ) ;
#10298 = CIRCLE ( 'NONE', #11006, 6.543750000000017053 ) ;
#10299 = DIRECTION ( 'NONE',  ( -1.000000000000000000, -7.703719777548943412E-32, 0.000000000000000000 ) ) ;
#10300 = ORIENTED_EDGE ( 'NONE', *, *, #6631, .F. ) ;
#10301 = FACE_OUTER_BOUND ( 'NONE', #5581, .T. ) ;
#10302 = STYLED_ITEM ( 'NONE', ( #4707 ), #1883 ) ;
#10303 = DIRECTION ( 'NONE',  ( 0.000000000000000000, 0.000000000000000000, -1.000000000000000000 ) ) ;
#10304 = CARTESIAN_POINT ( 'NONE',  ( -65.00000000000000000, -10.00000000000000178, 12.49999999999999467 ) ) ;
#10305 = EDGE_CURVE ( 'NONE', #18509, #23413, #19404, .T. ) ;
#10306 = EDGE_LOOP ( 'NONE', ( #7111, #11899, #6928, #6768 ) ) ;
#10307 = CARTESIAN_POINT ( 'NONE',  ( -3.999999999999999112, 1.656854249492380582, 14.06250000273119660 ) ) ;
#10308 = CARTESIAN_POINT ( 'NONE',  ( 71.40000000109249356, 7.933012699999995476, 15.85617417291294196 ) ) ;
#10309 = CARTESIAN_POINT ( 'NONE',  ( 0.000000000000000000, 0.000000000000000000, -4.974599999999998801 ) ) ;
#10310 = ORIENTED_EDGE ( 'NONE', *, *, #8035, .F. ) ;
#10311 = CARTESIAN_POINT ( 'NONE',  ( 4.999999999999999112, 4.729683950898872169, 7.360373001730934561 ) ) ;
#10312 = VERTEX_POINT ( 'NONE', #17750 ) ;
#10313 = CIRCLE ( 'NONE', #10702, 6.500000000000000888 ) ;
#10314 = CARTESIAN_POINT ( 'NONE',  ( -2.828427124746189403, 2.828427124746190291, 17.87500000000001066 ) ) ;
#10315 = CARTESIAN_POINT ( 'NONE',  ( 70.85000000218494165, 12.50000000000000000, 16.03553390593273420 ) ) ;
#10316 = CARTESIAN_POINT ( 'NONE',  ( 0.000000000000000000, 0.000000000000000000, 3.059999999999998277 ) ) ;
#10317 = AXIS2_PLACEMENT_3D ( 'NONE', #17120, #15109, #15348 ) ;
#10318 = CARTESIAN_POINT ( 'NONE',  ( -3.680118525130244400, 2.494084732383327285, -0.3507732604232449702 ) ) ;
#10319 = CARTESIAN_POINT ( 'NONE',  ( 66.55000000109247082, 11.46158073645647235, 16.46158073645647235 ) ) ;
#10320 = VERTEX_POINT ( 'NONE', #15953 ) ;
#10321 = DIRECTION ( 'NONE',  ( 0.000000000000000000, 0.000000000000000000, -1.000000000000000000 ) ) ;
#10322 = CARTESIAN_POINT ( 'NONE',  ( 50.00000000000000000, -14.69846310392956745, 35.82846581308617573 ) ) ;
#10323 = VECTOR ( 'NONE', #19503, 1000.000000000000114 ) ;
#10324 = CARTESIAN_POINT ( 'NONE',  ( 69.80000000109247082, 10.85617417291294551, 17.06698729999999742 ) ) ;
#10325 = CARTESIAN_POINT ( 'NONE',  ( 1.025207404391860050E-15, 3.458734125000000326, 11.18750000136560452 ) ) ;
#10326 = DIRECTION ( 'NONE',  ( 0.000000000000000000, 0.000000000000000000, 1.000000000000000000 ) ) ;
#10327 = VECTOR ( 'NONE', #17097, 1000.000000000000000 ) ;
#10328 = DIRECTION ( 'NONE',  ( 0.000000000000000000, 0.000000000000000000, 1.000000000000000000 ) ) ;
#10329 = ORIENTED_EDGE ( 'NONE', *, *, #22325, .T. ) ;
#10330 = FACE_OUTER_BOUND ( 'NONE', #20604, .T. ) ;
#10331 = CARTESIAN_POINT ( 'NONE',  ( 4.000000000000000888, 1.656854249492381248, 15.56250000000001066 ) ) ;
#10332 = CARTESIAN_POINT ( 'NONE',  ( 1.489200000000000079, 0.000000000000000000, 0.000000000000000000 ) ) ;
#10333 = CARTESIAN_POINT ( 'NONE',  ( 21.28513981966725765, -11.25000000000000355, 10.00000000000008882 ) ) ;
#10334 = ADVANCED_FACE ( 'NONE', ( #4928, #21671 ), #10822, .F. ) ;
#10335 = CARTESIAN_POINT ( 'NONE',  ( -2.117863837641485618E-16, 3.458734125000000326, -1.512499998634402987 ) ) ;
#10336 = EDGE_LOOP ( 'NONE', ( #2459, #7644, #13590, #10610 ) ) ;
#10337 = VECTOR ( 'NONE', #2633, 1000.000000000000000 ) ;
#10338 = ORIENTED_EDGE ( 'NONE', *, *, #18852, .T. ) ;
#10339 = CARTESIAN_POINT ( 'NONE',  ( -67.75000000109245946, 8.538419263543524096, 13.53841926354352054 ) ) ;
#10340 = ITEM_DEFINED_TRANSFORMATION ( 'NONE', 'NONE', #11873,  #7318 ) ;
#10341 = AXIS2_PLACEMENT_3D ( 'NONE', #14175, #8779, #13829 ) ;
#10342 = VERTEX_POINT ( 'NONE', #12378 ) ;
#10343 = FACE_OUTER_BOUND ( 'NONE', #22430, .T. ) ;
#10344 = EDGE_LOOP ( 'NONE', ( #19515, #16183, #10052, #15489 ) ) ;
#10345 = ORIENTED_EDGE ( 'NONE', *, *, #14311, .F. ) ;
#10346 = CARTESIAN_POINT ( 'NONE',  ( 2.445694354108821411, 2.445694354108820523, 11.31250000136560452 ) ) ;
#10347 = AXIS2_PLACEMENT_3D ( 'NONE', #23448, #7304, #8866 ) ;
#10348 = CARTESIAN_POINT ( 'NONE',  ( -3.028668353233801458, -9.000000000000005329, 10.00000000000008882 ) ) ;
#10349 = CIRCLE ( 'NONE', #21386, 8.749000000000002331 ) ;
#10350 = CYLINDRICAL_SURFACE ( 'NONE', #8313, 4.000000000000001776 ) ;
#10351 = CARTESIAN_POINT ( 'NONE',  ( 67.50000000109247367, 7.933012699999995476, 14.14382582708705094 ) ) ;
#10352 = CARTESIAN_POINT ( 'NONE',  ( -69.25000000000000000, 11.03553390593273598, 17.50000000000000355 ) ) ;
#10353 = DIRECTION ( 'NONE',  ( -0.000000000000000000, -0.000000000000000000, 1.000000000000000000 ) ) ;
#10354 = CARTESIAN_POINT ( 'NONE',  ( 59.99999999999729283, 11.05913360956146185, 18.21068369823747091 ) ) ;
#10355 = CARTESIAN_POINT ( 'NONE',  ( -3.458734125000000770, 0.000000000000000000, 0.9875000013655956810 ) ) ;
#10356 = CARTESIAN_POINT ( 'NONE',  ( 0.000000000000000000, 0.000000000000000000, 19.04999999999996874 ) ) ;
#10357 = CARTESIAN_POINT ( 'NONE',  ( -31.74999999999995737, 0.000000000000000000, 0.000000000000000000 ) ) ;
#10358 = CARTESIAN_POINT ( 'NONE',  ( -2.445694354108819191, 2.445694354108820523, 18.31250000136560274 ) ) ;
#10359 = DIRECTION ( 'NONE',  ( 0.000000000000000000, 0.000000000000000000, -1.000000000000000000 ) ) ;
#10360 = CIRCLE ( 'NONE', #3830, 4.000000000000001776 ) ;
#10361 = AXIS2_PLACEMENT_3D ( 'NONE', #20107, #12743, #16429 ) ;
#10362 = ORIENTED_EDGE ( 'NONE', *, *, #20233, .T. ) ;
#10363 = CARTESIAN_POINT ( 'NONE',  ( -9.000000000000000000, 1.102182119232617714E-15, -3.999999999999999112 ) ) ;
#10364 = ORIENTED_EDGE ( 'NONE', *, *, #6331, .F. ) ;
#10365 = CARTESIAN_POINT ( 'NONE',  ( 52.46643183416157541, 7.028187705514638672, 13.68930817193508531 ) ) ;
#10366 = CARTESIAN_POINT ( 'NONE',  ( -69.15000000109247935, 8.538419263543524096, 13.53841926354352054 ) ) ;
#10367 = FACE_OUTER_BOUND ( 'NONE', #23324, .T. ) ;
#10368 = ORIENTED_EDGE ( 'NONE', *, *, #2229, .F. ) ;
#10369 = VECTOR ( 'NONE', #20084, 1000.000000000000000 ) ;
#10370 = CARTESIAN_POINT ( 'NONE',  ( 118.3095189484530181, -15.00000000000003375, 34.11836509645780779 ) ) ;
#10371 = VECTOR ( 'NONE', #20941, 1000.000000000000000 ) ;
#10372 = ORIENTED_EDGE ( 'NONE', *, *, #8484, .T. ) ;
#10373 = DIRECTION ( 'NONE',  ( -1.000000000000000000, -0.000000000000000000, -0.000000000000000000 ) ) ;
#10374 = VERTEX_POINT ( 'NONE', #19644 ) ;
#10375 = CARTESIAN_POINT ( 'NONE',  ( 55.53356816583845301, 11.31069182806492712, 17.97181229448534623 ) ) ;
#10376 = ADVANCED_FACE ( 'NONE', ( #16080 ), #16193, .T. ) ;
#10377 = CARTESIAN_POINT ( 'NONE',  ( -65.90000000218495302, 11.76776695296636888, 13.23223304703362579 ) ) ;
#10378 =( BOUNDED_CURVE ( )  B_SPLINE_CURVE ( 2, ( #13882, #17810, #22831, #4753, #12089, #21377, #8716, #17347, #2829 ),
 .UNSPECIFIED., .F., .F. ) 
 B_SPLINE_CURVE_WITH_KNOTS ( ( 3, 2, 2, 2, 3 ),
 ( 0.5625000000000008882, 0.5781250000000007772, 0.5937500000000006661, 0.6093750000000006661, 0.6250000000000005551 ),
 .UNSPECIFIED. ) 
 CURVE ( )  GEOMETRIC_REPRESENTATION_ITEM ( )  RATIONAL_B_SPLINE_CURVE ( ( 0.9999999999999956701, 0.9238795325112910684, 1.000000000000000000, 0.9238795325112867385, 1.000000000000000000, 0.9238795325112867385, 1.000000000000000000, 0.9238795325112840739, 1.000000000000002665 ) ) 
 REPRESENTATION_ITEM ( '' )  );
#10379 = CARTESIAN_POINT ( 'NONE',  ( -3.251184232703611343, 2.330193357860981251, -3.674599999999999866 ) ) ;
#10380 = DIRECTION ( 'NONE',  ( -1.000000000000000000, -0.000000000000000000, -0.000000000000000000 ) ) ;
#10381 = CARTESIAN_POINT ( 'NONE',  ( -3.458734124999998105, -1.432654583217642497, 15.75000000136560629 ) ) ;
#10382 = CARTESIAN_POINT ( 'NONE',  ( -3.999999999999999112, 1.656854249492380804, 13.06250000273119660 ) ) ;
#10383 = EDGE_CURVE ( 'NONE', #21471, #16245, #23367, .T. ) ;
#10384 = CARTESIAN_POINT ( 'NONE',  ( 59.25000000000000711, 7.878679656440361612, 17.12132034355964549 ) ) ;
#10385 = AXIS2_PLACEMENT_3D ( 'NONE', #13436, #9472, #4305 ) ;
#10386 = DIRECTION ( 'NONE',  ( -7.087422195345011518E-32, -1.000000000000000000, -0.000000000000000000 ) ) ;
#10387 = LINE ( 'NONE', #22681, #8043 ) ;
#10388 = COLOUR_RGB ( '', 0.40784314, 0.44705882, 0.49803922) ;
#10389 = CARTESIAN_POINT ( 'NONE',  ( 58.12500000000000000, 12.12132034355964727, 17.12132034355963484 ) ) ;
#10390 = CARTESIAN_POINT ( 'NONE',  ( 1.432654583217640276, 3.458734125000000770, 0.6750000013655963471 ) ) ;
#10391 = CARTESIAN_POINT ( 'NONE',  ( 1.872352939448454495E-15, -3.458734125000000770, 12.93750000136560629 ) ) ;
#10392 = CARTESIAN_POINT ( 'NONE',  ( 19.57733605323380743, -9.000000000000003553, 5.000000000000079936 ) ) ;
#10393 = CARTESIAN_POINT ( 'NONE',  ( -67.70000000109247651, 7.933012699999995476, 14.14382582708705094 ) ) ;
#10394 = EDGE_LOOP ( 'NONE', ( #7226, #5011, #5595, #1481 ) ) ;
#10395 = DIRECTION ( 'NONE',  ( 0.3420201433256622736, 0.9396926207859106484, 0.000000000000000000 ) ) ;
#10396 = CARTESIAN_POINT ( 'NONE',  ( -4.235886605889389145, -2.417314728048544303, -3.751161874094020909 ) ) ;
#10397 = ORIENTED_EDGE ( 'NONE', *, *, #252, .T. ) ;
#10398 = CARTESIAN_POINT ( 'NONE',  ( 58.87500000000000711, 7.878679656440349177, 12.87867965644035984 ) ) ;
#10399 = CARTESIAN_POINT ( 'NONE',  ( 4.000000000000000888, -1.656854249492379694, -1.137499997268811125 ) ) ;
#10400 = EDGE_LOOP ( 'NONE', ( #10601, #9005, #6471, #6627 ) ) ;
#10401 = ORIENTED_EDGE ( 'NONE', *, *, #4205, .T. ) ;
#10402 = CARTESIAN_POINT ( 'NONE',  ( 1.599999999999998979, 8.073750000000021743, 0.000000000000000000 ) ) ;
#10403 = DIRECTION ( 'NONE',  ( -1.000000000000000000, 0.000000000000000000, -0.000000000000000000 ) ) ;
#10404 = ORIENTED_EDGE ( 'NONE', *, *, #20775, .F. ) ;
#10405 = DIRECTION ( 'NONE',  ( -0.000000000000000000, 0.000000000000000000, -1.000000000000000000 ) ) ;
#10406 = AXIS2_PLACEMENT_3D ( 'NONE', #9842, #19380, #22989 ) ;
#10407 = ADVANCED_FACE ( 'NONE', ( #14171 ), #1317, .T. ) ;
#10408 = CARTESIAN_POINT ( 'NONE',  ( -69.60000000218495586, 7.499999999999996447, 14.99999999999999645 ) ) ;
#10409 = EDGE_CURVE ( 'NONE', #8640, #20363, #1433, .T. ) ;
#10410 = CARTESIAN_POINT ( 'NONE',  ( -5.555405146766190683, -9.000000000000005329, 10.00000000000008882 ) ) ;
#10411 = CARTESIAN_POINT ( 'NONE',  ( 69.65000000109246514, 12.06698730000000097, 14.99999999999999645 ) ) ;
#10412 = EDGE_CURVE ( 'NONE', #17390, #17065, #3002, .T. ) ;
#10413 = DIRECTION ( 'NONE',  ( -0.000000000000000000, 0.000000000000000000, -1.000000000000000000 ) ) ;
#10414 =( BOUNDED_CURVE ( )  B_SPLINE_CURVE ( 2, ( #11521, #15695, #19249, #15344, #18901, #8146, #11867, #4175, #9706 ),
 .UNSPECIFIED., .F., .F. ) 
 B_SPLINE_CURVE_WITH_KNOTS ( ( 3, 2, 2, 2, 3 ),
 ( 0.7500000000000000000, 0.7624999999999999556, 0.7750000000000000222, 0.7874999999999999778, 0.8000000000000000444 ),
 .UNSPECIFIED. ) 
 CURVE ( )  GEOMETRIC_REPRESENTATION_ITEM ( )  RATIONAL_B_SPLINE_CURVE ( ( 1.000000000000000000, 0.9238795325112867385, 1.000000000000000000, 0.9238795325112867385, 1.000000000000000000, 0.9238795325112867385, 1.000000000000000000, 0.9238795325112867385, 1.000000000000000000 ) ) 
 REPRESENTATION_ITEM ( '' )  );
#10415 = DIRECTION ( 'NONE',  ( 0.000000000000000000, -0.8090169943749403458, -0.5877852522924831291 ) ) ;
#10416 = CARTESIAN_POINT ( 'NONE',  ( 56.18981816583843170, 9.931948859054346102, 10.99999999999999467 ) ) ;
#10417 = CARTESIAN_POINT ( 'NONE',  ( -1.432654583217640942, -3.458734124999999882, 4.925000001365594571 ) ) ;
#10418 = CARTESIAN_POINT ( 'NONE',  ( 1.025207404391860050E-15, 3.458734125000000326, 15.18750000136560452 ) ) ;
#10419 = DIRECTION ( 'NONE',  ( 0.3420201433256622181, 0.9396926207859107594, -6.162975822039141593E-32 ) ) ;
#10420 = CARTESIAN_POINT ( 'NONE',  ( -90.00000000000000000, 0.000000000000000000, -6.735000000000022524 ) ) ;
#10421 = ORIENTED_EDGE ( 'NONE', *, *, #6933, .T. ) ;
#10422 = CARTESIAN_POINT ( 'NONE',  ( -3.265986985212536720, 1.709698821660321499, 2.039999999999996927 ) ) ;
#10423 = CARTESIAN_POINT ( 'NONE',  ( 21.00000000000000355, 0.000000000000000000, 0.000000000000000000 ) ) ;
#10424 = CARTESIAN_POINT ( 'NONE',  ( -60.00000000000000711, -10.00000000000000178, 14.99999999999999467 ) ) ;
#10425 = ORIENTED_EDGE ( 'NONE', *, *, #8798, .T. ) ;
#10426 = DIRECTION ( 'NONE',  ( -1.000000000000000000, 0.000000000000000000, 0.000000000000000000 ) ) ;
#10427 = DIRECTION ( 'NONE',  ( 0.000000000000000000, 0.000000000000000000, 1.000000000000000000 ) ) ;
#10428 = EDGE_CURVE ( 'NONE', #6932, #12149, #1560, .T. ) ;
#10429 = FACE_OUTER_BOUND ( 'NONE', #818, .T. ) ;
#10430 = ORIENTED_EDGE ( 'NONE', *, *, #4646, .F. ) ;
#10431 = CYLINDRICAL_SURFACE ( 'NONE', #5684, 4.714285714285714413 ) ;
#10432 = ORIENTED_EDGE ( 'NONE', *, *, #15851, .T. ) ;
#10433 = CARTESIAN_POINT ( 'NONE',  ( 58.25231816583843170, 7.219692298483957771, 17.87654654797633924 ) ) ;
#10434 = EDGE_CURVE ( 'NONE', #12663, #16821, #22904, .T. ) ;
#10435 = CARTESIAN_POINT ( 'NONE',  ( 67.35000000218495586, 8.964466094067258695, 12.49999999999999289 ) ) ;
#10436 = CARTESIAN_POINT ( 'NONE',  ( -3.999999999999999112, 0.000000000000000000, 19.00000000000001066 ) ) ;
#10437 = CARTESIAN_POINT ( 'NONE',  ( -3.999999999999999112, 1.656854249492380582, 11.93750000000001066 ) ) ;
#10438 = CARTESIAN_POINT ( 'NONE',  ( 68.90000000109246514, 12.06698729999999919, 15.85617417291294196 ) ) ;
#10439 = EDGE_CURVE ( 'NONE', #3743, #5362, #6474, .T. ) ;
#10440 = ORIENTED_EDGE ( 'NONE', *, *, #20798, .F. ) ;
#10441 = EDGE_CURVE ( 'NONE', #13567, #7146, #21367, .T. ) ;
#10442 = CARTESIAN_POINT ( 'NONE',  ( 4.000000000000000000, 0.000000000000000000, 19.04999999999996874 ) ) ;
#10443 = DIRECTION ( 'NONE',  ( 0.3420201433256622181, -0.9396926207859107594, 0.000000000000000000 ) ) ;
#10444 = CARTESIAN_POINT ( 'NONE',  ( 67.90000000109245093, 10.85617417291294551, 12.93301269999999370 ) ) ;
#10445 = CARTESIAN_POINT ( 'NONE',  ( -2.445694354108819191, 2.445694354108820523, 11.31250000136560452 ) ) ;
#10446 = CARTESIAN_POINT ( 'NONE',  ( 4.999999999999999112, -6.772677083992345359, -5.538577986808975062 ) ) ;
#10447 = CARTESIAN_POINT ( 'NONE',  ( -6.500000000000000000, -3.142418015001830600, -3.295638806298776036 ) ) ;
#10448 = ORIENTED_EDGE ( 'NONE', *, *, #17973, .T. ) ;
#10449 = CARTESIAN_POINT ( 'NONE',  ( 2.828427124746190735, -2.828427124746189847, -1.324999999999997957 ) ) ;
#10450 = CARTESIAN_POINT ( 'NONE',  ( 57.18750000000000000, 9.999999999999989342, 11.99999999999999467 ) ) ;
#10451 = CARTESIAN_POINT ( 'NONE',  ( 2.000000000000001776, 8.130889342088981965E-16, -6.543750000000017053 ) ) ;
#10452 = VECTOR ( 'NONE', #569, 1000.000000000000000 ) ;
#10453 = EDGE_LOOP ( 'NONE', ( #992, #9857, #22524, #10397 ) ) ;
#10454 = CARTESIAN_POINT ( 'NONE',  ( 1.999999999999999112, 8.800000000000023803, 0.000000000000000000 ) ) ;
#10455 = CARTESIAN_POINT ( 'NONE',  ( 25.00005080000000035, 5.400000000000000355, 1.000000000000000000 ) ) ;
#10456 = VERTEX_POINT ( 'NONE', #23604 ) ;
#10457 = CARTESIAN_POINT ( 'NONE',  ( -1.520000000000000462, 0.000000000000000000, 0.000000000000000000 ) ) ;
#10458 = VERTEX_POINT ( 'NONE', #15848 ) ;
#10459 = DIRECTION ( 'NONE',  ( 0.000000000000000000, 0.000000000000000000, -1.000000000000000000 ) ) ;
#10460 = VERTEX_POINT ( 'NONE', #7218 ) ;
#10461 = CARTESIAN_POINT ( 'NONE',  ( 3.458734125000001658, 1.432654583217640498, 13.25000000136560452 ) ) ;
#10462 = CARTESIAN_POINT ( 'NONE',  ( 51.28125000000000000, 8.757359312880703683, 11.99999999999999822 ) ) ;
#10463 = DIRECTION ( 'NONE',  ( 0.3420201433256622736, -0.9396926207859106484, -1.232595164407828100E-31 ) ) ;
#10464 = CARTESIAN_POINT ( 'NONE',  ( 66.20000000109247651, 12.06698729999999919, 14.14382582708705094 ) ) ;
#10465 = EDGE_CURVE ( 'NONE', #7262, #20390, #5597, .T. ) ;
#10466 = CARTESIAN_POINT ( 'NONE',  ( -19.99999999999999645, -9.000000000000003553, 5.000000000000079936 ) ) ;
#10467 = EDGE_CURVE ( 'NONE', #13655, #7935, #18741, .T. ) ;
#10468 = CARTESIAN_POINT ( 'NONE',  ( -70.05000000000002558, 11.03553390593273598, 17.50000000000000355 ) ) ;
#10469 = CARTESIAN_POINT ( 'NONE',  ( -3.349226789952655547, -2.685125164760744809, -0.2236248678334863682 ) ) ;
#10470 = LINE ( 'NONE', #10823, #18485 ) ;
#10471 = CARTESIAN_POINT ( 'NONE',  ( 3.458734125000000770, 1.432654583217640498, -1.449999998634403653 ) ) ;
#10472 = CARTESIAN_POINT ( 'NONE',  ( 1.971781867644420635E-15, -4.000000000000000000, 13.25000000000001243 ) ) ;
#10473 = CARTESIAN_POINT ( 'NONE',  ( 19.99999999999998934, -9.999999999999964473, -50.00000000000000000 ) ) ;
#10474 = CARTESIAN_POINT ( 'NONE',  ( 1.432654583217643163, -3.458734124999999437, 15.75000000136560629 ) ) ;
#10475 = LINE ( 'NONE', #1324, #3838 ) ;
#10476 = ORIENTED_EDGE ( 'NONE', *, *, #3730, .F. ) ;
#10477 = CARTESIAN_POINT ( 'NONE',  ( 4.000000000000001776, -1.656854249492379694, 14.56250000273119660 ) ) ;
#10478 = VERTEX_POINT ( 'NONE', #20466 ) ;
#10479 = CARTESIAN_POINT ( 'NONE',  ( 59.31018183416157541, 14.00000000000000000, 15.06805114094561304 ) ) ;
#10480 = CARTESIAN_POINT ( 'NONE',  ( -66.30000000109247082, 12.06698730000000275, 15.85617417291294196 ) ) ;
#10481 = DIRECTION ( 'NONE',  ( -1.118373553621254909E-32, -0.9073324201775117004, -0.4204139380358592470 ) ) ;
#10482 = CARTESIAN_POINT ( 'NONE',  ( 27.50000000000000000, 4.500000000000001776, -33.66025403784446723 ) ) ;
#10483 = ORIENTED_EDGE ( 'NONE', *, *, #20431, .F. ) ;
#10484 = CARTESIAN_POINT ( 'NONE',  ( 4.688305830332750723, -11.25000000000000355, 5.000000000000079936 ) ) ;
#10485 = CONICAL_SURFACE ( 'NONE', #3558, 4.000000000000000000, 0.8911886515913786111 ) ;
#10486 = AXIS2_PLACEMENT_3D ( 'NONE', #8081, #17166, #8189 ) ;
#10487 = ORIENTED_EDGE ( 'NONE', *, *, #12762, .T. ) ;
#10488 = DIRECTION ( 'NONE',  ( 0.9396926207859107594, -0.3420201433256623291, 3.697785493223492838E-32 ) ) ;
#10489 = VERTEX_POINT ( 'NONE', #10934 ) ;
#10490 = CARTESIAN_POINT ( 'NONE',  ( 51.31481816583844591, 14.00000000000000178, 14.93194885905434610 ) ) ;
#10491 = CARTESIAN_POINT ( 'NONE',  ( -68.55000000218495870, 11.03553390593273598, 17.50000000000000355 ) ) ;
#10492 = CARTESIAN_POINT ( 'NONE',  ( 2.499999999999999556, -10.82112760146737962, 1.975651141462196225 ) ) ;
#10493 = PLANE ( 'NONE',  #11071 ) ;
#10494 = CARTESIAN_POINT ( 'NONE',  ( 2.445694354108821411, 2.445694354108820523, 17.31250000136560629 ) ) ;
#10495 = CARTESIAN_POINT ( 'NONE',  ( 2.828427124746191179, 2.828427124746190291, 10.75000000273119660 ) ) ;
#10496 = CARTESIAN_POINT ( 'NONE',  ( 57.28125000000000711, 8.757359312880703683, 11.99999999999999822 ) ) ;
#10497 = DIRECTION ( 'NONE',  ( -1.000000000000000000, -0.000000000000000000, -0.000000000000000000 ) ) ;
#10498 = AXIS2_PLACEMENT_3D ( 'NONE', #5456, #16839, #13138 ) ;
#10499 = CARTESIAN_POINT ( 'NONE',  ( 57.00000000000000000, 12.12132034355963484, 12.87867965644034740 ) ) ;
#10500 = PRODUCT_DEFINITION ( 'UNKNOWN', '', #18712, #18642 ) ;
#10501 = CARTESIAN_POINT ( 'NONE',  ( -1.432654583217641164, -3.458734125000000326, 2.175000001365597679 ) ) ;
#10502 = CARTESIAN_POINT ( 'NONE',  ( 1.125461230421587633, -3.270501301980698550, 2.040000000000001812 ) ) ;
#10503 = FACE_OUTER_BOUND ( 'NONE', #12857, .T. ) ;
#10504 = EDGE_CURVE ( 'NONE', #14810, #1264, #11047, .T. ) ;
#10505 = ORIENTED_EDGE ( 'NONE', *, *, #1635, .T. ) ;
#10506 = DIRECTION ( 'NONE',  ( 0.3420201433256622181, 0.9396926207859107594, -6.162975822039141593E-32 ) ) ;
#10507 = DIRECTION ( 'NONE',  ( 0.000000000000000000, 0.000000000000000000, 1.000000000000000000 ) ) ;
#10508 = ORIENTED_EDGE ( 'NONE', *, *, #14245, .F. ) ;
#10509 = DIRECTION ( 'NONE',  ( 1.000000000000000000, 0.000000000000000000, 0.000000000000000000 ) ) ;
#10510 = CARTESIAN_POINT ( 'NONE',  ( -2.828427124746190291, 2.828427124746190291, -1.699999997268811569 ) ) ;
#10511 = DIRECTION ( 'NONE',  ( 1.000000000000000000, 0.000000000000000000, 0.000000000000000000 ) ) ;
#10512 = ORIENTED_EDGE ( 'NONE', *, *, #15530, .T. ) ;
#10513 = ORIENTED_EDGE ( 'NONE', *, *, #12082, .F. ) ;
#10514 = FACE_BOUND ( 'NONE', #6169, .T. ) ;
#10515 = AXIS2_PLACEMENT_3D ( 'NONE', #12120, #6598, #2978 ) ;
#10516 =( BOUNDED_CURVE ( )  B_SPLINE_CURVE ( 2, ( #13357, #14925, #7603, #5793, #11204, #5911, #7835, #15156, #18367 ),
 .UNSPECIFIED., .F., .F. ) 
 B_SPLINE_CURVE_WITH_KNOTS ( ( 3, 2, 2, 2, 3 ),
 ( 0.3749999999999998890, 0.3906249999999997780, 0.4062499999999996669, 0.4218749999999996114, 0.4374999999999995004 ),
 .UNSPECIFIED. ) 
 CURVE ( )  GEOMETRIC_REPRESENTATION_ITEM ( )  RATIONAL_B_SPLINE_CURVE ( ( 1.000000000000000444, 0.9238795325112861834, 1.000000000000000000, 0.9238795325112867385, 1.000000000000000000, 0.9238795325112867385, 1.000000000000000000, 0.9238795325112891810, 0.9999999999999975575 ) ) 
 REPRESENTATION_ITEM ( '' )  );
#10517 = DIRECTION ( 'NONE',  ( 0.000000000000000000, 0.3090169943749481174, -0.9510565162951533091 ) ) ;
#10518 = ORIENTED_EDGE ( 'NONE', *, *, #6931, .T. ) ;
#10519 = CARTESIAN_POINT ( 'NONE',  ( -0.1410422978106123659, 4.700232962125094893, -3.687027686973624707 ) ) ;
#10520 = CARTESIAN_POINT ( 'NONE',  ( -69.65000000218496723, 7.499999999999996447, 13.96446609406725514 ) ) ;
#10521 = ORIENTED_EDGE ( 'NONE', *, *, #12913, .T. ) ;
#10522 = VECTOR ( 'NONE', #17406, 1000.000000000000114 ) ;
#10523 = CARTESIAN_POINT ( 'NONE',  ( -18.12177574676618974, -9.000000000000003553, 5.000000000000079936 ) ) ;
#10524 = B_SPLINE_CURVE_WITH_KNOTS ( 'NONE', 3,
 ( #11758, #10197, #19260, #3094, #22980 ),
 .UNSPECIFIED., .F., .F.,
 ( 4, 1, 4 ),
 ( 0.000000000000000000, 0.002309401076758505356, 0.004618802153517010713 ),
 .UNSPECIFIED. ) ;
#10525 = CARTESIAN_POINT ( 'NONE',  ( 71.54999999999999716, 12.50000000000000000, 16.03553390593273420 ) ) ;
#10526 = CARTESIAN_POINT ( 'NONE',  ( 4.999999999999999112, 9.241976615262160522, -1.699438267350405818 ) ) ;
#10528 = DIRECTION ( 'NONE',  ( 0.000000000000000000, 0.000000000000000000, -1.000000000000000000 ) ) ;
#10527 = AXIS2_PLACEMENT_3D ( 'NONE', #13835, #20855, #21090 ) ;
#10529 = CARTESIAN_POINT ( 'NONE',  ( 51.75000000000000711, 7.171572875253819923, 17.82842712474619873 ) ) ;
#10530 = CARTESIAN_POINT ( 'NONE',  ( -2.117863837641485618E-16, 3.458734125000000326, 3.487500001365594571 ) ) ;
#10531 = CARTESIAN_POINT ( 'NONE',  ( 2.445694354108821411, 2.445694354108820523, 15.06250000136560452 ) ) ;
#10532 = DIRECTION ( 'NONE',  ( 0.000000000000000000, 0.000000000000000000, 1.000000000000000000 ) ) ;
#10533 = EDGE_CURVE ( 'NONE', #12546, #15256, #12967, .T. ) ;
#10534 = DIRECTION ( 'NONE',  ( -1.000000000000000000, 0.000000000000000000, 0.000000000000000000 ) ) ;
#10535 = ORIENTED_EDGE ( 'NONE', *, *, #12913, .F. ) ;
#10536 = CARTESIAN_POINT ( 'NONE',  ( -1.594879469667249916, -11.25000000000000355, 5.000000000000079936 ) ) ;
#10537 = EDGE_CURVE ( 'NONE', #6430, #589, #11174, .T. ) ;
#10538 = DIRECTION ( 'NONE',  ( 1.000000000000000000, 0.000000000000000000, -0.000000000000000000 ) ) ;
#10539 = CARTESIAN_POINT ( 'NONE',  ( -65.00000000000000000, 9.999999999999998224, 17.49999999999999645 ) ) ;
#10540 = VERTEX_POINT ( 'NONE', #5513 ) ;
#10541 = DIRECTION ( 'NONE',  ( -1.000000000000000000, 0.000000000000000000, -0.000000000000000000 ) ) ;
#10542 = CARTESIAN_POINT ( 'NONE',  ( -67.70000000000000284, 9.999999999999998224, 17.49999999999999645 ) ) ;
#10543 = EDGE_CURVE ( 'NONE', #10566, #21201, #13378, .T. ) ;
#10544 = FACE_OUTER_BOUND ( 'NONE', #3444, .T. ) ;
#10545 = ORIENTED_EDGE ( 'NONE', *, *, #4767, .F. ) ;
#10546 = CARTESIAN_POINT ( 'NONE',  ( -68.45000000218495018, 12.50000000000000000, 16.03553390593273775 ) ) ;
#10547 = VERTEX_POINT ( 'NONE', #15120 ) ;
#10548 = VECTOR ( 'NONE', #23673, 1000.000000000000000 ) ;
#10549 = CARTESIAN_POINT ( 'NONE',  ( 59.00231816583843170, 12.78030770151603868, 12.12345345202365188 ) ) ;
#10550 = TOROIDAL_SURFACE ( 'NONE', #1336, 8.239200000000002078, 0.03079999999999879709 ) ;
#10551 = AXIS2_PLACEMENT_3D ( 'NONE', #13672, #4551, #11888 ) ;
#10552 = CARTESIAN_POINT ( 'NONE',  ( 68.40000000218495302, 12.50000000000000000, 14.99999999999999645 ) ) ;
#10553 = DIRECTION ( 'NONE',  ( -1.000000000000000000, -0.000000000000000000, -0.000000000000000000 ) ) ;
#10554 = CARTESIAN_POINT ( 'NONE',  ( -20.00005080000000035, 0.000000000000000000, 0.000000000000000000 ) ) ;
#10555 = CARTESIAN_POINT ( 'NONE',  ( 4.000000000000000000, 4.898587196589412829E-16, -0.1999999999999987899 ) ) ;
#10556 = ORIENTED_EDGE ( 'NONE', *, *, #1272, .T. ) ;
#10557 = CARTESIAN_POINT ( 'NONE',  ( 0.000000000000000000, 0.000000000000000000, 0.000000000000000000 ) ) ;
#10558 = EDGE_CURVE ( 'NONE', #2314, #3785, #11565, .T. ) ;
#10559 = DIRECTION ( 'NONE',  ( 0.000000000000000000, 0.000000000000000000, 1.000000000000000000 ) ) ;
#10560 = CARTESIAN_POINT ( 'NONE',  ( 67.55000000109247082, 8.538419263543522320, 16.46158073645647235 ) ) ;
#10561 = CARTESIAN_POINT ( 'NONE',  ( 2.445694354108822299, -2.445694354108820079, 18.06250000136560274 ) ) ;
#10562 = CARTESIAN_POINT ( 'NONE',  ( -14.98018309676618998, -9.000000000000003553, 10.00000000000008882 ) ) ;
#10563 = EDGE_CURVE ( 'NONE', #701, #9531, #9257, .T. ) ;
#10564 = VECTOR ( 'NONE', #21778, 1000.000000000000114 ) ;
#10565 = DIRECTION ( 'NONE',  ( -6.938893903907210234E-15, 0.000000000000000000, 1.000000000000000000 ) ) ;
#10566 = VERTEX_POINT ( 'NONE', #5634 ) ;
#10567 = CARTESIAN_POINT ( 'NONE',  ( -2.828427124746190291, 2.828427124746190291, -2.824999999999997513 ) ) ;
#10568 = EDGE_CURVE ( 'NONE', #10092, #12579, #4071, .T. ) ;
#10569 = CARTESIAN_POINT ( 'NONE',  ( 56.25000000000000711, 7.878679656440361612, 17.12132034355964549 ) ) ;
#10570 = AXIS2_PLACEMENT_3D ( 'NONE', #21140, #8599, #10532 ) ;
#10571 = CARTESIAN_POINT ( 'NONE',  ( 6.500000000000000000, -3.752776749732574135, -3.700000000000000178 ) ) ;
#10572 = DIRECTION ( 'NONE',  ( 1.000000000000000000, 7.703719777548943412E-32, 0.000000000000000000 ) ) ;
#10573 = ORIENTED_EDGE ( 'NONE', *, *, #12757, .T. ) ;
#10574 = CARTESIAN_POINT ( 'NONE',  ( 20.39626908033275043, -11.25000000000000355, 10.00000000000008882 ) ) ;
#10575 = CARTESIAN_POINT ( 'NONE',  ( -1.432654583217640276, 3.458734125000000326, -2.449999998634404097 ) ) ;
#10576 = LINE ( 'NONE', #21656, #17783 ) ;
#10577 = ADVANCED_FACE ( 'NONE', ( #14885 ), #5760, .T. ) ;
#10578 = ORIENTED_EDGE ( 'NONE', *, *, #5962, .T. ) ;
#10579 = ORIENTED_EDGE ( 'NONE', *, *, #5696, .F. ) ;
#10580 = ADVANCED_FACE ( 'NONE', ( #18560 ), #3594, .T. ) ;
#10581 = CARTESIAN_POINT ( 'NONE',  ( 2.828427124746191179, 2.828427124746190291, 12.75000000273119660 ) ) ;
#10582 = ORIENTED_EDGE ( 'NONE', *, *, #7963, .F. ) ;
#10583 = CARTESIAN_POINT ( 'NONE',  ( 9.920644283265380691E-16, 4.000000000000000000, 17.75000000000000711 ) ) ;
#10584 = CARTESIAN_POINT ( 'NONE',  ( -66.15000000000000568, 8.964466094067260471, 17.50000000000000355 ) ) ;
#10585 = VECTOR ( 'NONE', #11427, 1000.000000000000000 ) ;
#10586 = CARTESIAN_POINT ( 'NONE',  ( -66.65000000218496723, 11.03553390593276973, 12.50000000000002665 ) ) ;
#10587 = CONICAL_SURFACE ( 'NONE', #10951, 6.500000000000000888, 1.047197551196596521 ) ;
#10588 = DIRECTION ( 'NONE',  ( 0.000000000000000000, 0.000000000000000000, -1.000000000000000000 ) ) ;
#10589 = CARTESIAN_POINT ( 'NONE',  ( -2.804994570502171047, -3.229033611042465335, -3.526374918436838701 ) ) ;
#10590 = CARTESIAN_POINT ( 'NONE',  ( -70.34999999999999432, 7.499999999999995559, 13.96446609406725692 ) ) ;
#10591 = DIRECTION ( 'NONE',  ( -1.000000000000000000, 0.000000000000000000, 0.000000000000000000 ) ) ;
#10592 = CARTESIAN_POINT ( 'NONE',  ( 60.00000000000001421, 13.59380198783558669, 16.55161943776040800 ) ) ;
#10593 = CARTESIAN_POINT ( 'NONE',  ( 3.458734125000000770, 4.235727675282972223E-16, -0.5124999986344038749 ) ) ;
#10594 = CARTESIAN_POINT ( 'NONE',  ( 5.577176569667260608, -11.25000000000000355, 10.00000000000008882 ) ) ;
#10595 = EDGE_CURVE ( 'NONE', #16281, #1668, #12619, .T. ) ;
#10596 = LINE ( 'NONE', #16199, #5757 ) ;
#10597 = CARTESIAN_POINT ( 'NONE',  ( -3.458734124999998993, 1.432654583217640276, 18.37500000136560274 ) ) ;
#10598 = DIRECTION ( 'NONE',  ( 0.000000000000000000, 0.000000000000000000, 1.000000000000000000 ) ) ;
#10599 = EDGE_LOOP ( 'NONE', ( #3231, #17560 ) ) ;
#10600 = DIRECTION ( 'NONE',  ( -0.3373062947069096484, 0.9413949561959079615, 0.000000000000000000 ) ) ;
#10601 = ORIENTED_EDGE ( 'NONE', *, *, #20338, .F. ) ;
#10602 = CARTESIAN_POINT ( 'NONE',  ( 59.21643183416158962, 13.97181229448536399, 16.72490539043799629 ) ) ;
#10603 = CARTESIAN_POINT ( 'NONE',  ( -67.60000000109248219, 9.143825827087050939, 12.93301269999999370 ) ) ;
#10604 = DIRECTION ( 'NONE',  ( -1.118373553621255183E-32, 0.9073324201775119224, 0.4204139380358593581 ) ) ;
#10605 = EDGE_CURVE ( 'NONE', #3718, #23046, #17179, .T. ) ;
#10606 = LINE ( 'NONE', #21686, #20858 ) ;
#10607 = VERTEX_POINT ( 'NONE', #2273 ) ;
#10608 = CARTESIAN_POINT ( 'NONE',  ( -71.40000000218495302, 9.999999999999998224, 12.49999999999999289 ) ) ;
#10609 = EDGE_CURVE ( 'NONE', #2153, #22848, #23278, .T. ) ;
#10610 = ORIENTED_EDGE ( 'NONE', *, *, #3635, .F. ) ;
#10611 = PLANE ( 'NONE',  #17543 ) ;
#10612 = VERTEX_POINT ( 'NONE', #16427 ) ;
#10613 = CARTESIAN_POINT ( 'NONE',  ( 51.78356816583844591, 8.689308171935074654, 12.02818770551464489 ) ) ;
#10614 = CARTESIAN_POINT ( 'NONE',  ( -68.20000000218495018, 9.999999999999998224, 12.49999999999999289 ) ) ;
#10615 = DIRECTION ( 'NONE',  ( 0.3420201433256622181, 0.9396926207859107594, -6.162975822039141593E-32 ) ) ;
#10616 = DIRECTION ( 'NONE',  ( 0.000000000000000000, 0.000000000000000000, -1.000000000000000000 ) ) ;
#10617 = CARTESIAN_POINT ( 'NONE',  ( -3.458734124999998105, -1.432654583217642497, 14.75000000136560452 ) ) ;
#10618 = DIRECTION ( 'NONE',  ( 0.000000000000000000, 0.000000000000000000, 1.000000000000000000 ) ) ;
#10619 = CARTESIAN_POINT ( 'NONE',  ( 56.43750000000000000, 10.00000000000000711, 17.99999999999999645 ) ) ;
#10620 = DIRECTION ( 'NONE',  ( 0.000000000000000000, 1.000000000000000000, 3.491481338843133355E-15 ) ) ;
#10621 = CARTESIAN_POINT ( 'NONE',  ( 57.65625000000002132, 7.000000000000003553, 16.24264068711929099 ) ) ;
#10622 = CARTESIAN_POINT ( 'NONE',  ( -3.458734125000000770, 0.000000000000000000, -0.01249999863440348635 ) ) ;
#10623 = DIRECTION ( 'NONE',  ( 0.000000000000000000, 0.000000000000000000, -1.000000000000000000 ) ) ;
#10624 = DIRECTION ( 'NONE',  ( 0.000000000000000000, 0.4999999999999990008, -0.8660254037844391517 ) ) ;
#10625 = ORIENTED_EDGE ( 'NONE', *, *, #22199, .T. ) ;
#10626 = CARTESIAN_POINT ( 'NONE',  ( 0.000000000000000000, 0.000000000000000000, 1.734723475976807094E-15 ) ) ;
#10627 = CARTESIAN_POINT ( 'NONE',  ( -3.453038570459499024, -2.625189405340453419, -3.535263753545272891 ) ) ;
#10628 = ORIENTED_EDGE ( 'NONE', *, *, #23560, .T. ) ;
#10629 = CARTESIAN_POINT ( 'NONE',  ( 57.93750000000000000, 10.00000000000000711, 17.99999999999999645 ) ) ;
#10630 = CARTESIAN_POINT ( 'NONE',  ( 4.000000000000000000, 1.656854249492381248, 1.987500002731187765 ) ) ;
#10631 = EDGE_CURVE ( 'NONE', #22912, #6574, #14647, .T. ) ;
#10632 = PLANE ( 'NONE',  #5178 ) ;
#10633 = ORIENTED_EDGE ( 'NONE', *, *, #7894, .F. ) ;
#10634 = VERTEX_POINT ( 'NONE', #3707 ) ;
#10635 = FILL_AREA_STYLE_COLOUR ( '', #6800 ) ;
#10636 = DIRECTION ( 'NONE',  ( -1.000000000000000000, 0.000000000000000000, 0.000000000000000000 ) ) ;
#10637 = EDGE_LOOP ( 'NONE', ( #8917, #6607, #4677, #14188, #18038, #1780, #22331, #6111, #6545, #545, #18726, #952, #10535, #9255, #20890, #22456, #18984, #19861, #22982, #22192, #7549, #15855, #1096, #4851, #11526, #9499, #15478, #11307, #15310, #12073, #6937, #2096, #16560, #3855, #9786, #7515, #6865, #15666, #17139, #10102, #6013, #3690, #10364, #22327, #18313, #10117, #13792, #1046, #12420, #6090, #4654, #14712, #5450, #4171, #3097, #18433, #13980, #5912, #20696, #22028, #221, #20839, #8612, #10978, #16498, #9757, #11959, #755, #4496, #23170, #20626, #14474, #10759, #14998, #16026, #22248, #5872, #2316, #10119, #19708, #15074, #21893, #3254, #6229, #19661 ) ) ;
#10638 = CIRCLE ( 'NONE', #2944, 8.749000000000002331 ) ;
#10639 = DIRECTION ( 'NONE',  ( -1.000000000000000000, -0.000000000000000000, -0.000000000000000000 ) ) ;
#10640 = ORIENTED_EDGE ( 'NONE', *, *, #18126, .T. ) ;
#10641 = CARTESIAN_POINT ( 'NONE',  ( 4.000000000000000000, 0.3987449864460005378, -0.01220643443059817035 ) ) ;
#10642 = CONICAL_SURFACE ( 'NONE', #20156, 6.500000000000000888, 1.047197551196596521 ) ;
#10643 = VECTOR ( 'NONE', #13659, 1000.000000000000114 ) ;
#10644 = CARTESIAN_POINT ( 'NONE',  ( 71.05000000000001137, 7.499999999999995559, 16.03553390593273420 ) ) ;
#10645 = CARTESIAN_POINT ( 'NONE',  ( -65.75000000218494733, 8.964466094067219615, 12.50000000000003553 ) ) ;
#10646 = LINE ( 'NONE', #5103, #14553 ) ;
#10647 = CARTESIAN_POINT ( 'NONE',  ( 58.90856816583844591, 13.97181229448534978, 13.27509460956196641 ) ) ;
#10648 = CARTESIAN_POINT ( 'NONE',  ( -1.432654583217640942, -3.458734124999999882, 2.925000001365598123 ) ) ;
#10649 = PRESENTATION_STYLE_ASSIGNMENT (( #8966 ) ) ;
#10650 = CARTESIAN_POINT ( 'NONE',  ( 3.458734125000001214, 4.235727675282971730E-16, 15.93750000136560629 ) ) ;
#10651 = FACE_OUTER_BOUND ( 'NONE', #21711, .T. ) ;
#10652 = VECTOR ( 'NONE', #14613, 1000.000000000000000 ) ;
#10653 = CARTESIAN_POINT ( 'NONE',  ( 0.000000000000000000, -1.239665997526951724, 9.314797388894888286 ) ) ;
#10654 = VERTEX_POINT ( 'NONE', #8161 ) ;
#10655 = CARTESIAN_POINT ( 'NONE',  ( 0.000000000000000000, 0.000000000000000000, -0.3080913168122742518 ) ) ;
#10656 =( BOUNDED_CURVE ( )  B_SPLINE_CURVE ( 2, ( #15667, #2573, #661, #898, #21127, #4499, #22815, #13745, #9793 ),
 .UNSPECIFIED., .F., .F. ) 
 B_SPLINE_CURVE_WITH_KNOTS ( ( 3, 2, 2, 2, 3 ),
 ( 0.3499999999999999778, 0.3624999999999999889, 0.3750000000000000000, 0.3875000000000000111, 0.4000000000000000222 ),
 .UNSPECIFIED. ) 
 CURVE ( )  GEOMETRIC_REPRESENTATION_ITEM ( )  RATIONAL_B_SPLINE_CURVE ( ( 1.000000000000000000, 0.9238795325112867385, 1.000000000000000000, 0.9238795325112867385, 1.000000000000000000, 0.9238795325112867385, 1.000000000000000000, 0.9238795325112867385, 1.000000000000000000 ) ) 
 REPRESENTATION_ITEM ( '' )  );
#10657 = DIRECTION ( 'NONE',  ( 0.000000000000000000, 0.000000000000000000, 1.000000000000000000 ) ) ;
#10658 = DIRECTION ( 'NONE',  ( -1.224646799147353207E-16, 0.000000000000000000, -1.000000000000000000 ) ) ;
#10659 = ORIENTED_EDGE ( 'NONE', *, *, #16158, .T. ) ;
#10660 = DIRECTION ( 'NONE',  ( 0.000000000000000000, 0.3090169943749412895, 0.9510565162951556406 ) ) ;
#10661 = VERTEX_POINT ( 'NONE', #5992 ) ;
#10662 = DIRECTION ( 'NONE',  ( 1.000000000000000000, 0.000000000000000000, 0.000000000000000000 ) ) ;
#10663 = ORIENTED_EDGE ( 'NONE', *, *, #6728, .T. ) ;
#10664 = DIRECTION ( 'NONE',  ( -1.000000000000000000, 0.000000000000000000, 0.000000000000000000 ) ) ;
#10665 = EDGE_LOOP ( 'NONE', ( #1497, #22938, #21816, #21782 ) ) ;
#10666 = CARTESIAN_POINT ( 'NONE',  ( 52.78125000000000711, 8.343145750507600766, 11.00000000000000533 ) ) ;
#10667 = CARTESIAN_POINT ( 'NONE',  ( 68.10000000218495586, 8.232233047033629347, 13.23223304703362402 ) ) ;
#10668 = EDGE_CURVE ( 'NONE', #22004, #4764, #18328, .T. ) ;
#10669 = DIRECTION ( 'NONE',  ( 0.3420201433256622181, 0.9396926207859107594, -6.162975822039141593E-32 ) ) ;
#10670 = LINE ( 'NONE', #17947, #21308 ) ;
#10671 = DIRECTION ( 'NONE',  ( 0.000000000000000000, 0.000000000000000000, 1.000000000000000000 ) ) ;
#10672 = ORIENTED_EDGE ( 'NONE', *, *, #16855, .F. ) ;
#10673 = CIRCLE ( 'NONE', #3372, 4.000000000000001776 ) ;
#10674 = CARTESIAN_POINT ( 'NONE',  ( 1.411581201560190495E-15, 4.862606272033091592, -3.745885042887436622 ) ) ;
#10675 = CARTESIAN_POINT ( 'NONE',  ( 57.52893183416158962, 11.58880310854676132, 19.02818770551463956 ) ) ;
#10676 = CARTESIAN_POINT ( 'NONE',  ( 27.50000000000000000, 4.500000000000006217, -33.66025403784446723 ) ) ;
#10677 = ADVANCED_FACE ( 'NONE', ( #8394 ), #11764, .F. ) ;
#10678 = CARTESIAN_POINT ( 'NONE',  ( 67.45000000109246230, 9.999999999999998224, 17.06698730000000097 ) ) ;
#10679 = CARTESIAN_POINT ( 'NONE',  ( 1.025207404391860050E-15, 3.458734125000000770, 17.43750000136560274 ) ) ;
#10680 = CYLINDRICAL_SURFACE ( 'NONE', #15887, 4.000000000000001776 ) ;
#10681 = DIRECTION ( 'NONE',  ( -7.087422195345011518E-32, -1.000000000000000000, -0.000000000000000000 ) ) ;
#10682 = ORIENTED_EDGE ( 'NONE', *, *, #4335, .F. ) ;
#10683 = FACE_OUTER_BOUND ( 'NONE', #12838, .T. ) ;
#10684 = CARTESIAN_POINT ( 'NONE',  ( 58.40625000000000711, 12.99999999999999645, 13.75735931288070191 ) ) ;
#10685 = CARTESIAN_POINT ( 'NONE',  ( 2.828427124746191179, 2.828427124746190291, 10.75000000273119660 ) ) ;
#10686 = DIRECTION ( 'NONE',  ( 0.000000000000000000, 0.000000000000000000, 1.000000000000000000 ) ) ;
#10687 = ORIENTED_EDGE ( 'NONE', *, *, #4541, .T. ) ;
#10688 = AXIS2_PLACEMENT_3D ( 'NONE', #1464, #12291, #3032 ) ;
#10689 = CARTESIAN_POINT ( 'NONE',  ( -19.99999999999999645, -9.000000000000003553, 5.000000000000079936 ) ) ;
#10690 = CARTESIAN_POINT ( 'NONE',  ( 3.458734125000000326, 4.235727675282971730E-16, -1.762499998634403209 ) ) ;
#10691 = CARTESIAN_POINT ( 'NONE',  ( -3.999999999999999112, 0.000000000000000000, 21.31370849898476649 ) ) ;
#10692 = EDGE_LOOP ( 'NONE', ( #7939, #7682, #18034, #13360 ) ) ;
#10693 = ORIENTED_EDGE ( 'NONE', *, *, #23667, .T. ) ;
#10694 = VECTOR ( 'NONE', #796, 1000.000000000000000 ) ;
#10695 = CARTESIAN_POINT ( 'NONE',  ( 2.828427124746191179, 2.828427124746190291, 19.62500000000001066 ) ) ;
#10696 = DIRECTION ( 'NONE',  ( -1.000000000000000000, 0.000000000000000000, 0.000000000000000000 ) ) ;
#10697 = EDGE_CURVE ( 'NONE', #17674, #7114, #17351, .T. ) ;
#10698 = CARTESIAN_POINT ( 'NONE',  ( 21.28513981966725765, -11.25000000000000355, 10.00000000000008882 ) ) ;
#10699 = ADVANCED_FACE ( 'NONE', ( #17490 ), #2852, .T. ) ;
#10700 = AXIS2_PLACEMENT_3D ( 'NONE', #21306, #5403, #5046 ) ;
#10701 = CARTESIAN_POINT ( 'NONE',  ( 51.00000000000000711, 12.82842712474617741, 12.17157287525379239 ) ) ;
#10702 = AXIS2_PLACEMENT_3D ( 'NONE', #17546, #8925, #14074 ) ;
#10703 = CARTESIAN_POINT ( 'NONE',  ( -67.39999999999999147, 11.76776695296636888, 13.23223304703362579 ) ) ;
#10704 = B_SPLINE_CURVE_WITH_KNOTS ( 'NONE', 3,
 ( #20571, #6220, #13782, #4178, #11986, #11871 ),
 .UNSPECIFIED., .F., .F.,
 ( 4, 2, 4 ),
 ( 2.380733003126162433E-07, 0.001898835937927379836, 0.003797433802554446743 ),
 .UNSPECIFIED. ) ;
#10705 = CARTESIAN_POINT ( 'NONE',  ( 66.60000000218495586, 9.999999999999998224, 12.49999999999999289 ) ) ;
#10706 = ADVANCED_FACE ( 'NONE', ( #7917 ), #11536, .F. ) ;
#10707 = CARTESIAN_POINT ( 'NONE',  ( 55.00000000000000711, 15.00000000000000000, 10.00000000000000000 ) ) ;
#10708 = EDGE_CURVE ( 'NONE', #7114, #1597, #17134, .T. ) ;
#10709 = VECTOR ( 'NONE', #5091, 1000.000000000000114 ) ;
#10710 = CARTESIAN_POINT ( 'NONE',  ( -3.458734125000000770, 1.432654583217640498, -0.07499999863440427739 ) ) ;
#10711 = CARTESIAN_POINT ( 'NONE',  ( 67.15000000218495302, 7.499999999999996447, 16.03553390593273775 ) ) ;
#10712 = CARTESIAN_POINT ( 'NONE',  ( 68.45000000218495018, 12.50000000000000000, 16.03553390593273775 ) ) ;
#10713 = CARTESIAN_POINT ( 'NONE',  ( 1.872352939448454495E-15, -3.458734125000000326, 16.68750000136560629 ) ) ;
#10714 = CARTESIAN_POINT ( 'NONE',  ( -66.40000000218495302, 7.499999999999996447, 14.99999999999999645 ) ) ;
#10715 = VERTEX_POINT ( 'NONE', #18806 ) ;
#10716 = CARTESIAN_POINT ( 'NONE',  ( -71.35000000109246798, 8.538419263543522320, 16.46158073645647235 ) ) ;
#10717 = VERTEX_POINT ( 'NONE', #20932 ) ;
#10718 = CARTESIAN_POINT ( 'NONE',  ( 56.77893183416158251, 8.411196891453236901, 10.97181229448535511 ) ) ;
#10719 = CARTESIAN_POINT ( 'NONE',  ( -68.70000000109246230, 12.06698730000000275, 15.85617417291294196 ) ) ;
#10720 = DIRECTION ( 'NONE',  ( 6.123233995736766036E-17, 1.000000000000000000, 0.000000000000000000 ) ) ;
#10721 = AXIS2_PLACEMENT_3D ( 'NONE', #3944, #22136, #5752 ) ;
#10722 = DIRECTION ( 'NONE',  ( 0.000000000000000000, 0.000000000000000000, 1.000000000000000000 ) ) ;
#10723 = ORIENTED_EDGE ( 'NONE', *, *, #10956, .T. ) ;
#10724 = CARTESIAN_POINT ( 'NONE',  ( -4.000000000000000000, 0.000000000000000000, -2.699999999999999289 ) ) ;
#10725 = AXIS2_PLACEMENT_3D ( 'NONE', #23337, #6946, #19852 ) ;
#10726 = EDGE_CURVE ( 'NONE', #3902, #17992, #710, .T. ) ;
#10727 = ORIENTED_EDGE ( 'NONE', *, *, #16537, .F. ) ;
#10728 = CARTESIAN_POINT ( 'NONE',  ( 71.04999999999999716, 7.499999999999996447, 16.03553390593273775 ) ) ;
#10729 = VERTEX_POINT ( 'NONE', #6114 ) ;
#10730 = CARTESIAN_POINT ( 'NONE',  ( 59.81250000000000711, 13.00000000000000000, 14.99999999999998757 ) ) ;
#10731 = CARTESIAN_POINT ( 'NONE',  ( -71.55000000109247082, 8.538419263543524096, 13.53841926354352054 ) ) ;
#10732 = AXIS2_PLACEMENT_3D ( 'NONE', #20656, #6183, #4372 ) ;
#10733 = ADVANCED_FACE ( 'NONE', ( #19155 ), #8000, .T. ) ;
#10734 = DIRECTION ( 'NONE',  ( -1.000000000000000000, 0.000000000000000000, 1.224646799147353207E-16 ) ) ;
#10735 = CARTESIAN_POINT ( 'NONE',  ( 0.000000000000000000, -9.915734732513184824, -4.762163868918378284 ) ) ;
#10736 = CARTESIAN_POINT ( 'NONE',  ( 1.025207404391860050E-15, 3.458734125000000770, 16.43750000136560629 ) ) ;
#10737 = CARTESIAN_POINT ( 'NONE',  ( 2.828427124746192067, -2.828427124746189847, 11.50000000273119660 ) ) ;
#10738 = EDGE_CURVE ( 'NONE', #15974, #18572, #4548, .T. ) ;
#10739 = CARTESIAN_POINT ( 'NONE',  ( 56.06250000000000000, 6.999999999999997335, 15.00000000000000533 ) ) ;
#10740 = DIRECTION ( 'NONE',  ( 1.000000000000000000, 0.000000000000000000, -9.637352644315595243E-17 ) ) ;
#10741 = VECTOR ( 'NONE', #10847, 1000.000000000000114 ) ;
#10742 = EDGE_CURVE ( 'NONE', #10755, #19924, #13444, .T. ) ;
#10743 = AXIS2_PLACEMENT_3D ( 'NONE', #8246, #2939, #23178 ) ;
#10744 = CARTESIAN_POINT ( 'NONE',  ( 52.06481816583844591, 6.999999999999998224, 15.06805114094563436 ) ) ;
#10745 = DIRECTION ( 'NONE',  ( 0.000000000000000000, 0.000000000000000000, 1.000000000000000000 ) ) ;
#10746 = CARTESIAN_POINT ( 'NONE',  ( 4.000000000000000888, 4.898587196589412829E-16, 18.62500000273119483 ) ) ;
#10747 = CARTESIAN_POINT ( 'NONE',  ( 70.45000000218495018, 7.499999999999996447, 13.96446609406725514 ) ) ;
#10748 = AXIS2_PLACEMENT_3D ( 'NONE', #15210, #6570, #13528 ) ;
#10749 = ORIENTED_EDGE ( 'NONE', *, *, #18837, .F. ) ;
#10750 = CARTESIAN_POINT ( 'NONE',  ( 23.53786173033275375, -11.25000000000000355, 5.000000000000079936 ) ) ;
#10751 = ORIENTED_EDGE ( 'NONE', *, *, #6266, .T. ) ;
#10752 = CARTESIAN_POINT ( 'NONE',  ( 53.81250000000000711, 13.00000000000000000, 14.99999999999998757 ) ) ;
#10753 = CARTESIAN_POINT ( 'NONE',  ( 7.347880794884118750E-16, -4.000000000000000000, -0.3249999972688121241 ) ) ;
#10754 = DIRECTION ( 'NONE',  ( -6.779273404243054876E-32, -0.9396926207859083169, 0.3420201433256691015 ) ) ;
#10755 = VERTEX_POINT ( 'NONE', #2504 ) ;
#10756 = CARTESIAN_POINT ( 'NONE',  ( 1.656854249492384135, -3.999999999999999112, 18.31250000000001421 ) ) ;
#10757 = ORIENTED_EDGE ( 'NONE', *, *, #21797, .T. ) ;
#10758 = CARTESIAN_POINT ( 'NONE',  ( 69.05000000000002558, 12.50000000000000000, 13.96446609406725692 ) ) ;
#10759 = ORIENTED_EDGE ( 'NONE', *, *, #23074, .F. ) ;
#10760 = CYLINDRICAL_SURFACE ( 'NONE', #14536, 9.000000000000000000 ) ;
#10761 = CARTESIAN_POINT ( 'NONE',  ( 1.971781867644420635E-15, -4.000000000000000000, 12.25000000000001066 ) ) ;
#10762 = VERTEX_POINT ( 'NONE', #22742 ) ;
#10763 = CARTESIAN_POINT ( 'NONE',  ( 31.59224393136097930, 9.778041110016188142, 10.00000000000008882 ) ) ;
#10764 = CIRCLE ( 'NONE', #398, 4.000000000000000888 ) ;
#10765 = CARTESIAN_POINT ( 'NONE',  ( 70.64999999999999147, 12.50000000000000000, 13.96446609406725869 ) ) ;
#10766 = ADVANCED_FACE ( 'NONE', ( #21052 ), #18914, .T. ) ;
#10767 = LINE ( 'NONE', #18042, #7053 ) ;
#10768 = ADVANCED_FACE ( 'NONE', ( #15361, #22628 ), #6231, .F. ) ;
#10769 = CARTESIAN_POINT ( 'NONE',  ( 69.70000000218495018, 8.232233047033629347, 13.23223304703362402 ) ) ;
#10770 = CARTESIAN_POINT ( 'NONE',  ( 57.31481816583843170, 14.00000000000000178, 14.93194885905434610 ) ) ;
#10771 = CARTESIAN_POINT ( 'NONE',  ( -1.432654583217640276, 3.458734125000000326, 1.550000001365597013 ) ) ;
#10772 = CARTESIAN_POINT ( 'NONE',  ( 118.3095189484530181, -2.399706452296379577, 55.00000000000021316 ) ) ;
#10773 = CARTESIAN_POINT ( 'NONE',  ( -2.445694354108818303, -2.445694354108820523, 14.56250000136560452 ) ) ;
#10774 = CARTESIAN_POINT ( 'NONE',  ( -1.656854249492380138, -3.999999999999999112, 18.31250000273119483 ) ) ;
#10775 = CARTESIAN_POINT ( 'NONE',  ( 0.000000000000000000, 0.000000000000000000, -4.974599999999998801 ) ) ;
#10776 = ORIENTED_EDGE ( 'NONE', *, *, #9138, .T. ) ;
#10777 = CARTESIAN_POINT ( 'NONE',  ( -3.544972969423974440, -0.09312760838339886882, 2.039999999999999591 ) ) ;
#10778 = DIRECTION ( 'NONE',  ( 0.000000000000000000, 0.000000000000000000, 1.000000000000000000 ) ) ;
#10779 = CARTESIAN_POINT ( 'NONE',  ( -0.3649867057748643617, 3.983313282257324950, 10.00000000000000888 ) ) ;
#10780 = EDGE_LOOP ( 'NONE', ( #135, #9673, #1048, #5256 ) ) ;
#10781 = VERTEX_POINT ( 'NONE', #938 ) ;
#10782 = CARTESIAN_POINT ( 'NONE',  ( 4.999999999999999112, 0.000000000000000000, 0.000000000000000000 ) ) ;
#10783 = CARTESIAN_POINT ( 'NONE',  ( 4.999999999999999112, 8.264486777890107660, -4.472189673936815879 ) ) ;
#10784 = ORIENTED_EDGE ( 'NONE', *, *, #2370, .T. ) ;
#10785 = CARTESIAN_POINT ( 'NONE',  ( -3.999999999999999112, 0.000000000000000000, 16.12500000273119838 ) ) ;
#10786 = VERTEX_POINT ( 'NONE', #3459 ) ;
#10787 = CARTESIAN_POINT ( 'NONE',  ( 54.75000000000000711, 7.171572875253819923, 17.82842712474619873 ) ) ;
#10788 = CARTESIAN_POINT ( 'NONE',  ( 66.80000000218494449, 12.50000000000000000, 14.99999999999999645 ) ) ;
#10789 = PLANE ( 'NONE',  #10347 ) ;
#10790 = CARTESIAN_POINT ( 'NONE',  ( -3.847601380332740018, -11.25000000000000355, 5.000000000000079936 ) ) ;
#10791 = CARTESIAN_POINT ( 'NONE',  ( 1.799999999999999600, 1.077689183249673761E-15, 8.800000000000023803 ) ) ;
#10792 = VERTEX_POINT ( 'NONE', #21404 ) ;
#10793 = CARTESIAN_POINT ( 'NONE',  ( 4.000000000000000888, 1.656854249492381248, 16.68750000273119838 ) ) ;
#10794 = DIRECTION ( 'NONE',  ( -1.000000000000000000, -0.000000000000000000, 0.000000000000000000 ) ) ;
#10795 =( BOUNDED_CURVE ( )  B_SPLINE_CURVE ( 2, ( #8767, #3480, #18089, #21788, #16421, #6840, #12735, #10584, #19756 ),
 .UNSPECIFIED., .F., .F. ) 
 B_SPLINE_CURVE_WITH_KNOTS ( ( 3, 2, 2, 2, 3 ),
 ( 0.9375000000000007772, 0.9531250000000005551, 0.9687500000000004441, 0.9843750000000002220, 1.000000000000000000 ),
 .UNSPECIFIED. ) 
 CURVE ( )  GEOMETRIC_REPRESENTATION_ITEM ( )  RATIONAL_B_SPLINE_CURVE ( ( 0.9999999999999962252, 0.9238795325112905132, 1.000000000000000000, 0.9238795325112867385, 1.000000000000000000, 0.9238795325112867385, 1.000000000000000000, 0.9238795325112867385, 1.000000000000000000 ) ) 
 REPRESENTATION_ITEM ( '' )  );
#10796 = CARTESIAN_POINT ( 'NONE',  ( 53.59143183416158962, 11.31069182806491291, 12.02818770551463778 ) ) ;
#10797 = CARTESIAN_POINT ( 'NONE',  ( -3.019423509283438722, -8.974600000000002353, 5.000000000000079936 ) ) ;
#10798 = DIRECTION ( 'NONE',  ( -1.000000000000000000, 0.000000000000000000, 0.000000000000000000 ) ) ;
#10799 = CARTESIAN_POINT ( 'NONE',  ( -72.37500000054622262, 9.999999999999998224, 17.28349365000000049 ) ) ;
#10800 = CARTESIAN_POINT ( 'NONE',  ( 0.000000000000000000, 0.000000000000000000, 0.000000000000000000 ) ) ;
#10801 = ORIENTED_EDGE ( 'NONE', *, *, #20765, .T. ) ;
#10802 = CARTESIAN_POINT ( 'NONE',  ( 6.500000000000000000, 3.752776749732563477, -3.700000000000000178 ) ) ;
#10803 = PRODUCT_DEFINITION ( 'UNKNOWN', '', #20984, #8355 ) ;
#10804 = CARTESIAN_POINT ( 'NONE',  ( 59.62500000000000711, 12.12132034355964727, 17.12132034355963484 ) ) ;
#10805 = LINE ( 'NONE', #3221, #1657 ) ;
#10806 = DIRECTION ( 'NONE',  ( -1.000000000000000000, -0.000000000000000000, -0.000000000000000000 ) ) ;
#10807 = VERTEX_POINT ( 'NONE', #10322 ) ;
#10808 = EDGE_CURVE ( 'NONE', #3506, #17633, #23338, .T. ) ;
#10809 = CARTESIAN_POINT ( 'NONE',  ( 41.56848460323381289, -9.000000000000001776, 5.000000000000079936 ) ) ;
#10810 = CARTESIAN_POINT ( 'NONE',  ( -3.458734124999999882, -1.432654583217642497, -2.199999998634404541 ) ) ;
#10811 = LINE ( 'NONE', #6831, #4389 ) ;
#10812 = ORIENTED_EDGE ( 'NONE', *, *, #15246, .F. ) ;
#10813 = CARTESIAN_POINT ( 'NONE',  ( -6.259644161404860030E-16, -4.618802153517027165, -5.000000000000000000 ) ) ;
#10814 = ORIENTED_EDGE ( 'NONE', *, *, #9997, .F. ) ;
#10815 = CARTESIAN_POINT ( 'NONE',  ( -3.999999999999999112, 0.000000000000000000, 13.12500000273119660 ) ) ;
#10816 = CARTESIAN_POINT ( 'NONE',  ( -3.999999999999999112, 0.000000000000000000, 17.00000000000001066 ) ) ;
#10817 = DIRECTION ( 'NONE',  ( 0.000000000000000000, 1.000000000000000000, -1.287488025362403787E-15 ) ) ;
#10818 = DIRECTION ( 'NONE',  ( -0.000000000000000000, -1.000000000000000000, -0.000000000000000000 ) ) ;
#10819 = CARTESIAN_POINT ( 'NONE',  ( 4.000000000000000888, 4.898587196589412829E-16, 21.31370849898476649 ) ) ;
#10820 = DIRECTION ( 'NONE',  ( -0.000000000000000000, -0.000000000000000000, -1.000000000000000000 ) ) ;
#10821 = CARTESIAN_POINT ( 'NONE',  ( -66.40000000000000568, 8.232233047033629347, 13.23223304703362402 ) ) ;
#10822 = PLANE ( 'NONE',  #8066 ) ;
#10823 = CARTESIAN_POINT ( 'NONE',  ( -3.999999999999999112, 0.000000000000000000, 21.31370849898476649 ) ) ;
#10824 = DIRECTION ( 'NONE',  ( 0.000000000000000000, 0.000000000000000000, 1.000000000000000000 ) ) ;
#10825 = CARTESIAN_POINT ( 'NONE',  ( 4.000000000000000000, 1.656854249492381248, 5.862500000000002487 ) ) ;
#10826 = CARTESIAN_POINT ( 'NONE',  ( 2.828427124746190735, -2.828427124746189847, 0.6750000000000020428 ) ) ;
#10827 = LINE ( 'NONE', #14415, #4613 ) ;
#10828 = CARTESIAN_POINT ( 'NONE',  ( -3.458734124999998993, 1.432654583217640276, 16.37500000136560629 ) ) ;
#10829 = CARTESIAN_POINT ( 'NONE',  ( -1.600000000000004086, 0.000000000000000000, -6.735000000000022524 ) ) ;
#10830 = ORIENTED_EDGE ( 'NONE', *, *, #16060, .T. ) ;
#10831 = EDGE_CURVE ( 'NONE', #4495, #6890, #3212, .T. ) ;
#10832 = CARTESIAN_POINT ( 'NONE',  ( -71.80000000109247082, 12.06698729999999919, 14.14382582708705094 ) ) ;
#10833 = ORIENTED_EDGE ( 'NONE', *, *, #8370, .F. ) ;
#10834 = CARTESIAN_POINT ( 'NONE',  ( 53.12268183416157541, 12.78030770151606177, 17.87654654797631792 ) ) ;
#10835 = CARTESIAN_POINT ( 'NONE',  ( -68.15000000109247935, 8.538419263543522320, 16.46158073645647235 ) ) ;
#10836 = CARTESIAN_POINT ( 'NONE',  ( -27.50000000000000711, 12.49999999999999645, -33.66025403784446723 ) ) ;
#10837 = EDGE_CURVE ( 'NONE', #3012, #9892, #1651, .T. ) ;
#10838 = CARTESIAN_POINT ( 'NONE',  ( -2.117863837641485618E-16, 3.458734125000000326, -1.512499998634402987 ) ) ;
#10839 = ORIENTED_EDGE ( 'NONE', *, *, #16016, .F. ) ;
#10840 = EDGE_LOOP ( 'NONE', ( #5622, #12483 ) ) ;
#10841 = FACE_OUTER_BOUND ( 'NONE', #795, .T. ) ;
#10842 = EDGE_CURVE ( 'NONE', #5303, #4502, #8624, .T. ) ;
#10843 = CARTESIAN_POINT ( 'NONE',  ( 52.06481816583844591, 6.999999999999998224, 15.06805114094563436 ) ) ;
#10844 = CARTESIAN_POINT ( 'NONE',  ( -69.95000000109247651, 8.538419263543524096, 13.53841926354352054 ) ) ;
#10845 = CARTESIAN_POINT ( 'NONE',  ( -70.25000000109245946, 9.999999999999998224, 12.93301269999999192 ) ) ;
#10846 = CARTESIAN_POINT ( 'NONE',  ( -3.458734124999999437, 0.000000000000000000, 13.68750000136560629 ) ) ;
#10847 = DIRECTION ( 'NONE',  ( 0.3420201433256622181, 0.9396926207859107594, -6.162975822039141593E-32 ) ) ;
#10848 = CARTESIAN_POINT ( 'NONE',  ( 53.90625000000000000, 12.99999999999999645, 13.75735931288070191 ) ) ;
#10849 = CARTESIAN_POINT ( 'NONE',  ( -27.50000000000000711, 7.500000000000001776, -33.66025403784446723 ) ) ;
#10850 = CARTESIAN_POINT ( 'NONE',  ( 53.43750000000000711, 10.00000000000000711, 17.99999999999999645 ) ) ;
#10851 = CARTESIAN_POINT ( 'NONE',  ( 4.000000000000000888, 4.898587196589412829E-16, 15.62500000273119660 ) ) ;
#10852 = CARTESIAN_POINT ( 'NONE',  ( 2.499999999999999556, 1.975651141462390514, -10.82112760146734232 ) ) ;
#10853 = CIRCLE ( 'NONE', #20381, 8.749000000000002331 ) ;
#10854 = VERTEX_POINT ( 'NONE', #21643 ) ;
#10855 = FACE_OUTER_BOUND ( 'NONE', #20320, .T. ) ;
#10856 = FACE_OUTER_BOUND ( 'NONE', #8088, .T. ) ;
#10857 = ORIENTED_EDGE ( 'NONE', *, *, #13517, .F. ) ;
#10858 = CARTESIAN_POINT ( 'NONE',  ( 52.50000000000000711, 12.12132034355963484, 12.87867965644034740 ) ) ;
#10859 = CARTESIAN_POINT ( 'NONE',  ( 3.458734125000000326, 1.432654583217640498, 5.300000001365596347 ) ) ;
#10860 = EDGE_CURVE ( 'NONE', #3586, #1384, #8995, .T. ) ;
#10861 = DIRECTION ( 'NONE',  ( 0.9396926207859107594, -0.3420201433256623291, 3.697785493223492838E-32 ) ) ;
#10862 = ORIENTED_EDGE ( 'NONE', *, *, #17156, .F. ) ;
#10863 = CARTESIAN_POINT ( 'NONE',  ( 2.828427124746191179, 2.828427124746190291, 17.62500000000001066 ) ) ;
#10864 = ORIENTED_EDGE ( 'NONE', *, *, #2370, .F. ) ;
#10865 =( LENGTH_UNIT ( ) NAMED_UNIT ( * ) SI_UNIT ( .MILLI., .METRE. ) );
#10866 = CARTESIAN_POINT ( 'NONE',  ( 72.50000000000000000, 9.999999999999998224, 14.99999999999999645 ) ) ;
#10867 = ORIENTED_EDGE ( 'NONE', *, *, #19706, .T. ) ;
#10868 = ADVANCED_FACE ( 'NONE', ( #23204 ), #1400, .F. ) ;
#10869 = DIRECTION ( 'NONE',  ( 1.000000000000000000, -0.000000000000000000, 0.000000000000000000 ) ) ;
#10870 = ADVANCED_FACE ( 'NONE', ( #17612 ), #5132, .T. ) ;
#10871 = FACE_OUTER_BOUND ( 'NONE', #22475, .T. ) ;
#10872 = ORIENTED_EDGE ( 'NONE', *, *, #6434, .T. ) ;
#10873 = CARTESIAN_POINT ( 'NONE',  ( 65.75000000109247367, 8.538419263543522320, 16.46158073645647235 ) ) ;
#10874 = CARTESIAN_POINT ( 'NONE',  ( 72.39999999999999147, 11.76776695296636888, 16.76776695296636532 ) ) ;
#10875 = CARTESIAN_POINT ( 'NONE',  ( -1.065083781909173410, 6.890627091270371096, -3.442152416367929124 ) ) ;
#10876 = CARTESIAN_POINT ( 'NONE',  ( 69.29999999999999716, 9.999999999999998224, 17.49999999999999645 ) ) ;
#10877 = CARTESIAN_POINT ( 'NONE',  ( 51.46875000000000000, 5.999999999999987566, 13.34314575050763452 ) ) ;
#10878 = CARTESIAN_POINT ( 'NONE',  ( -2.445694354108820523, 2.445694354108820523, -1.387499998634402987 ) ) ;
#10879 = CARTESIAN_POINT ( 'NONE',  ( 12.17357108409515476, 2.710222204658223610, 10.00000000000008882 ) ) ;
#10880 = CARTESIAN_POINT ( 'NONE',  ( 1.872352939448454495E-15, -3.458734125000000326, 11.68750000136560629 ) ) ;
#10881 = DIRECTION ( 'NONE',  ( 0.000000000000000000, 0.000000000000000000, -1.000000000000000000 ) ) ;
#10882 = DIRECTION ( 'NONE',  ( 1.000000000000000000, 0.000000000000000000, 0.000000000000000000 ) ) ;
#10883 = ORIENTED_EDGE ( 'NONE', *, *, #12316, .F. ) ;
#10884 = CARTESIAN_POINT ( 'NONE',  ( -65.00000000000000000, -9.999999999999998224, 25.00000000000001421 ) ) ;
#10885 = DIRECTION ( 'NONE',  ( 0.000000000000000000, 0.000000000000000000, 1.000000000000000000 ) ) ;
#10886 = ORIENTED_EDGE ( 'NONE', *, *, #1042, .F. ) ;
#10887 = VERTEX_POINT ( 'NONE', #19854 ) ;
#10888 = LINE ( 'NONE', #23189, #7956 ) ;
#10889 = EDGE_CURVE ( 'NONE', #19904, #16384, #16423, .T. ) ;
#10890 = ADVANCED_FACE ( 'NONE', ( #22985 ), #14139, .T. ) ;
#10891 = CARTESIAN_POINT ( 'NONE',  ( 56.53125000000000711, 11.65685424949239923, 18.99999999999998934 ) ) ;
#10892 = ORIENTED_EDGE ( 'NONE', *, *, #14311, .T. ) ;
#10893 = LINE ( 'NONE', #11240, #17569 ) ;
#10894 = ORIENTED_EDGE ( 'NONE', *, *, #15921, .T. ) ;
#10895 = ADVANCED_FACE ( 'NONE', ( #8874 ), #5022, .T. ) ;
#10896 = CARTESIAN_POINT ( 'NONE',  ( 51.28125000000000000, 8.343145750507600766, 11.00000000000000533 ) ) ;
#10897 = CARTESIAN_POINT ( 'NONE',  ( 69.50000000218494733, 8.232233047033627571, 16.76776695296636532 ) ) ;
#10898 = LINE ( 'NONE', #18064, #6109 ) ;
#10899 = DIRECTION ( 'NONE',  ( -1.000000000000000000, -7.703719777548943412E-32, 0.000000000000000000 ) ) ;
#10900 = CARTESIAN_POINT ( 'NONE',  ( -4.000000000000000000, 2.309401076758498483, -5.000000000000000000 ) ) ;
#10901 = ORIENTED_EDGE ( 'NONE', *, *, #19557, .F. ) ;
#10903 = CARTESIAN_POINT ( 'NONE',  ( 4.000000000000000888, 4.898587196589412829E-16, 17.62500000273119483 ) ) ;
#10902 = B_SPLINE_CURVE_WITH_KNOTS ( 'NONE', 3,
 ( #8010, #2588, #9933, #11508, #18780, #21023 ),
 .UNSPECIFIED., .F., .F.,
 ( 4, 2, 4 ),
 ( 2.380733003329415929E-07, 0.001898835937927393280, 0.003797433802554453681 ),
 .UNSPECIFIED. ) ;
#10904 = DIRECTION ( 'NONE',  ( 0.000000000000000000, 0.000000000000000000, -1.000000000000000000 ) ) ;
#10905 = CARTESIAN_POINT ( 'NONE',  ( 60.34143183416158962, 8.275094609562001935, 18.97181229448536044 ) ) ;
#10906 = CARTESIAN_POINT ( 'NONE',  ( -2.117863837641483646E-16, 3.458734125000000770, -3.295601554149324208 ) ) ;
#10907 = CARTESIAN_POINT ( 'NONE',  ( 66.05000000109247082, 7.933012699999995476, 14.99999999999999645 ) ) ;
#10908 = CARTESIAN_POINT ( 'NONE',  ( 72.50000000000000000, 9.999999999999998224, 17.49999999999999645 ) ) ;
#10909 = CARTESIAN_POINT ( 'NONE',  ( -68.89999999999999147, 9.999999999999998224, 12.49999999999999289 ) ) ;
#10910 = EDGE_LOOP ( 'NONE', ( #23640, #6749, #13953, #11451 ) ) ;
#10911 = CARTESIAN_POINT ( 'NONE',  ( -20.00000000000001066, 9.999999999999964473, -49.99999999999999289 ) ) ;
#10912 = CARTESIAN_POINT ( 'NONE',  ( 56.34375000000000711, 8.757359312880723223, 18.00000000000000711 ) ) ;
#10913 = DIRECTION ( 'NONE',  ( 0.3420201433256622181, 0.9396926207859107594, -6.162975822039141593E-32 ) ) ;
#10914 =( LENGTH_UNIT ( ) NAMED_UNIT ( * ) SI_UNIT ( .MILLI., .METRE. ) );
#10915 = ORIENTED_EDGE ( 'NONE', *, *, #17141, .F. ) ;
#10916 = PLANE ( 'NONE',  #7089 ) ;
#10917 = DIRECTION ( 'NONE',  ( -7.087422195345011518E-32, -1.000000000000000000, -0.000000000000000000 ) ) ;
#10918 = FACE_OUTER_BOUND ( 'NONE', #18330, .T. ) ;
#10919 = VECTOR ( 'NONE', #19074, 1000.000000000000000 ) ;
#10920 = EDGE_CURVE ( 'NONE', #7848, #3586, #16048, .T. ) ;
#10921 = CIRCLE ( 'NONE', #18926, 4.000000000000001776 ) ;
#10922 = ORIENTED_EDGE ( 'NONE', *, *, #18195, .T. ) ;
#10923 = CYLINDRICAL_SURFACE ( 'NONE', #22106, 4.000000000000000000 ) ;
#10924 = VERTEX_POINT ( 'NONE', #14382 ) ;
#10925 = DIRECTION ( 'NONE',  ( -1.000000000000000000, 0.000000000000000000, 0.000000000000000000 ) ) ;
#10926 = CARTESIAN_POINT ( 'NONE',  ( 1.872352939448454495E-15, -3.458734125000000770, 10.93750000136560452 ) ) ;
#10927 = CARTESIAN_POINT ( 'NONE',  ( 42.38741763033275589, -11.25000000000000355, 5.000000000000079936 ) ) ;
#10928 = PLANE ( 'NONE',  #21384 ) ;
#10929 = DIRECTION ( 'NONE',  ( 1.000000000000000000, 0.000000000000000000, 0.000000000000000000 ) ) ;
#10930 = DIRECTION ( 'NONE',  ( 0.000000000000000000, 0.000000000000000000, 1.000000000000000000 ) ) ;
#10931 = AXIS2_PLACEMENT_3D ( 'NONE', #22611, #9946, #6214 ) ;
#10932 = DIRECTION ( 'NONE',  ( -1.000000000000000000, 0.000000000000000000, 0.000000000000000000 ) ) ;
#10933 = AXIS2_PLACEMENT_3D ( 'NONE', #23312, #15569, #23182 ) ;
#10934 = CARTESIAN_POINT ( 'NONE',  ( -1.647987302177966740E-14, -7.505553499465137612, -0.5805565836007695601 ) ) ;
#10935 = CARTESIAN_POINT ( 'NONE',  ( 3.458734125000001214, 4.235727675282971730E-16, 18.93750000136560629 ) ) ;
#10936 = CARTESIAN_POINT ( 'NONE',  ( -6.259644161404862988E-16, -4.618802153517027165, -3.504271511726793076 ) ) ;
#10937 = CARTESIAN_POINT ( 'NONE',  ( 1.656854249492383024, -3.999999999999999112, 3.612500000000005596 ) ) ;
#10938 = CARTESIAN_POINT ( 'NONE',  ( -1.970342311631612331, 3.497176594775547542, 10.00018359407915192 ) ) ;
#10939 = CARTESIAN_POINT ( 'NONE',  ( 3.458734125000001214, 4.235727675282971730E-16, 13.93750000136560629 ) ) ;
#10940 = CARTESIAN_POINT ( 'NONE',  ( 27.50000000000000000, 7.500000000000002665, -33.66025403784446723 ) ) ;
#10941 = ORIENTED_EDGE ( 'NONE', *, *, #2258, .F. ) ;
#10942 = CARTESIAN_POINT ( 'NONE',  ( -69.75000000109247367, 8.538419263543522320, 16.46158073645647235 ) ) ;
#10943 = ORIENTED_EDGE ( 'NONE', *, *, #7622, .F. ) ;
#10944 = CARTESIAN_POINT ( 'NONE',  ( 56.31018183416157541, 14.00000000000000000, 15.06805114094561304 ) ) ;
#10945 = CARTESIAN_POINT ( 'NONE',  ( -68.95000000109247651, 8.538419263543522320, 16.46158073645647235 ) ) ;
#10946 = DIRECTION ( 'NONE',  ( -1.000000000000000000, 0.000000000000000000, 0.000000000000000000 ) ) ;
#10947 = CARTESIAN_POINT ( 'NONE',  ( 72.50000000000000000, 9.999999999999998224, 17.49999999999999645 ) ) ;
#10948 = ORIENTED_EDGE ( 'NONE', *, *, #10742, .T. ) ;
#10949 = VECTOR ( 'NONE', #7936, 1000.000000000000114 ) ;
#10950 = ORIENTED_EDGE ( 'NONE', *, *, #19086, .F. ) ;
#10951 = AXIS2_PLACEMENT_3D ( 'NONE', #13644, #8251, #15570 ) ;
#10952 = CYLINDRICAL_SURFACE ( 'NONE', #15216, 7.000000000000000000 ) ;
#10953 = CARTESIAN_POINT ( 'NONE',  ( 53.47106816583843880, 6.971812294485350670, 13.82541045382635403 ) ) ;
#10954 = CARTESIAN_POINT ( 'NONE',  ( -71.70000000109247651, 10.85617417291294551, 12.93301269999999370 ) ) ;
#10955 = VECTOR ( 'NONE', #8167, 1000.000000000000000 ) ;
#10956 = EDGE_CURVE ( 'NONE', #15043, #6042, #4187, .T. ) ;
#10957 = CARTESIAN_POINT ( 'NONE',  ( -68.85000000109246798, 12.06698730000000097, 14.99999999999999645 ) ) ;
#10958 = CARTESIAN_POINT ( 'NONE',  ( 1.025207404391860050E-15, 3.458734125000000770, 10.43750000136560629 ) ) ;
#10959 = CARTESIAN_POINT ( 'NONE',  ( -3.999999999999999112, 0.000000000000000000, 10.12500000273119660 ) ) ;
#10960 = CARTESIAN_POINT ( 'NONE',  ( 52.12500000000000711, 12.12132034355964727, 17.12132034355963484 ) ) ;
#10961 = CARTESIAN_POINT ( 'NONE',  ( -0.1828748004095307189, 4.000000000000000000, 9.881898421846274871 ) ) ;
#10962 = CARTESIAN_POINT ( 'NONE',  ( 51.93750000000000711, 10.00000000000000711, 17.99999999999999645 ) ) ;
#10963 = FACE_OUTER_BOUND ( 'NONE', #42, .T. ) ;
#10964 = EDGE_CURVE ( 'NONE', #3670, #18990, #12235, .T. ) ;
#10965 = CARTESIAN_POINT ( 'NONE',  ( 2.500000000000000000, -2.357898499370432166, 3.035766082959412415E-15 ) ) ;
#10966 = ORIENTED_EDGE ( 'NONE', *, *, #19023, .T. ) ;
#10967 = DIRECTION ( 'NONE',  ( 0.000000000000000000, 0.000000000000000000, -1.000000000000000000 ) ) ;
#10968 = CARTESIAN_POINT ( 'NONE',  ( 44.70083240928345703, -8.974600000000002353, 5.000000000000079936 ) ) ;
#10969 = ORIENTED_EDGE ( 'NONE', *, *, #13812, .F. ) ;
#10970 = CARTESIAN_POINT ( 'NONE',  ( 54.56250000000000711, 6.999999999999997335, 15.00000000000000533 ) ) ;
#10971 = SHAPE_REPRESENTATION_RELATIONSHIP ( 'NONE' , 'NONE' ,  #20612, #19027 ) ;
#10972 = CARTESIAN_POINT ( 'NONE',  ( 1.656854249492383024, -3.999999999999999112, -3.262499997268812901 ) ) ;
#10973 = CARTESIAN_POINT ( 'NONE',  ( 50.00000000000000000, -2.399706452296379577, 55.00000000000021316 ) ) ;
#10974 = ORIENTED_EDGE ( 'NONE', *, *, #4930, .T. ) ;
#10975 = CARTESIAN_POINT ( 'NONE',  ( -2.828427124746188515, -2.828427124746190735, 16.12500000000001066 ) ) ;
#10976 = DIRECTION ( 'NONE',  ( 0.000000000000000000, 1.000000000000000000, -1.224646799147353207E-16 ) ) ;
#10977 = CARTESIAN_POINT ( 'NONE',  ( 69.14999999999999147, 12.50000000000000000, 16.03553390593273775 ) ) ;
#10978 = ORIENTED_EDGE ( 'NONE', *, *, #7740, .F. ) ;
#10979 = DIRECTION ( 'NONE',  ( 0.000000000000000000, -0.000000000000000000, -1.000000000000000000 ) ) ;
#10980 = CARTESIAN_POINT ( 'NONE',  ( 45.00000000000000711, -9.796556200126381952, 10.73275603335500072 ) ) ;
#10981 = CARTESIAN_POINT ( 'NONE',  ( -2.445694354108819635, -2.445694354108820967, 0.1125000013655966247 ) ) ;
#10982 = EDGE_CURVE ( 'NONE', #10073, #17999, #16168, .T. ) ;
#10983 = CARTESIAN_POINT ( 'NONE',  ( 69.99999999999998579, 11.76776695296636888, 16.76776695296636532 ) ) ;
#10984 = ADVANCED_FACE ( 'NONE', ( #17723 ), #14619, .F. ) ;
#10985 = CARTESIAN_POINT ( 'NONE',  ( 19.99999999999998934, 7.500000000000002665, -50.00000000000000000 ) ) ;
#10986 = CARTESIAN_POINT ( 'NONE',  ( 69.60000000218495586, 7.499999999999996447, 14.99999999999999645 ) ) ;
#10987 = CARTESIAN_POINT ( 'NONE',  ( 52.62731816583844591, 12.87654654797634102, 17.78030770151602979 ) ) ;
#10988 = CARTESIAN_POINT ( 'NONE',  ( 3.458734125000000326, 1.432654583217640498, -1.699999998634404097 ) ) ;
#10989 = EDGE_CURVE ( 'NONE', #21989, #19450, #23695, .T. ) ;
#10990 = CARTESIAN_POINT ( 'NONE',  ( 0.000000000000000000, 8.475820894093034852, -4.057423117305300586 ) ) ;
#10991 = EDGE_CURVE ( 'NONE', #15816, #19016, #2306, .T. ) ;
#10992 = CIRCLE ( 'NONE', #20126, 7.000000000000000000 ) ;
#10993 = CARTESIAN_POINT ( 'NONE',  ( -3.999999999999999112, 0.000000000000000000, 21.31370849898476649 ) ) ;
#10994 = ORIENTED_EDGE ( 'NONE', *, *, #7239, .T. ) ;
#10995 = CARTESIAN_POINT ( 'NONE',  ( 6.500000000000000000, -0.6341575537611440216, -3.700000000000001066 ) ) ;
#10996 = DIRECTION ( 'NONE',  ( 1.000000000000000000, -0.000000000000000000, -0.000000000000000000 ) ) ;
#10997 = CARTESIAN_POINT ( 'NONE',  ( -0.3649867057748917842, 3.983313282257320509, 9.889028792932920808 ) ) ;
#10998 = ORIENTED_EDGE ( 'NONE', *, *, #15009, .T. ) ;
#10999 = ORIENTED_EDGE ( 'NONE', *, *, #16710, .T. ) ;
#11000 = CARTESIAN_POINT ( 'NONE',  ( 2.500000000000000888, 3.061616997868384127E-16, -4.974599999999998801 ) ) ;
#11001 = ORIENTED_EDGE ( 'NONE', *, *, #2319, .T. ) ;
#11002 = CARTESIAN_POINT ( 'NONE',  ( 54.28125000000000000, 8.343145750507600766, 11.00000000000000355 ) ) ;
#11003 = ORIENTED_EDGE ( 'NONE', *, *, #22832, .T. ) ;
#11004 = DIRECTION ( 'NONE',  ( 0.000000000000000000, -0.7071067811865406894, 0.7071067811865545671 ) ) ;
#11005 = ORIENTED_EDGE ( 'NONE', *, *, #9496, .F. ) ;
#11006 = AXIS2_PLACEMENT_3D ( 'NONE', #6093, #4649, #8378 ) ;
#11007 = CARTESIAN_POINT ( 'NONE',  ( 53.75231816583844591, 7.219692298483957771, 17.87654654797633924 ) ) ;
#11008 = CARTESIAN_POINT ( 'NONE',  ( 72.00000000109248788, 10.85617417291294551, 17.06698729999999742 ) ) ;
#11009 = CARTESIAN_POINT ( 'NONE',  ( 60.00000000000000711, 12.82842712474617741, 12.17157287525379239 ) ) ;
#11010 = DIRECTION ( 'NONE',  ( 0.000000000000000000, 5.754033390038006453E-16, 1.000000000000000000 ) ) ;
#11011 = EDGE_CURVE ( 'NONE', #22026, #19360, #20198, .T. ) ;
#11012 = CARTESIAN_POINT ( 'NONE',  ( 43.27628836966725601, -11.25000000000000355, 5.000000000000079936 ) ) ;
#11013 = EDGE_LOOP ( 'NONE', ( #8528, #14965, #6453, #6084 ) ) ;
#11014 = CARTESIAN_POINT ( 'NONE',  ( 4.000000000000001776, -1.656854249492379694, 18.56250000273119838 ) ) ;
#11015 = AXIS2_PLACEMENT_3D ( 'NONE', #15980, #8680, #16536 ) ;
#11016 = CARTESIAN_POINT ( 'NONE',  ( 44.10446624071656174, -8.974600000000002353, 5.000000000000079936 ) ) ;
#11017 = CARTESIAN_POINT ( 'NONE',  ( 56.21643183416158251, 13.97181229448536399, 16.72490539043799629 ) ) ;
#11018 = DIRECTION ( 'NONE',  ( 1.000000000000000000, 7.703719777548943412E-32, 0.000000000000000000 ) ) ;
#11019 = FACE_OUTER_BOUND ( 'NONE', #21135, .T. ) ;
#11020 = VECTOR ( 'NONE', #16499, 1000.000000000000000 ) ;
#11021 = CARTESIAN_POINT ( 'NONE',  ( -68.89999999999999147, 9.999999999999998224, 12.49999999999999289 ) ) ;
#11022 = CIRCLE ( 'NONE', #2579, 9.000000000000023093 ) ;
#11023 = EDGE_CURVE ( 'NONE', #19235, #2236, #11143, .T. ) ;
#11024 = CARTESIAN_POINT ( 'NONE',  ( 4.197478902586992966, -0.8524102783748346290, -3.505063281295504041 ) ) ;
#11025 = ORIENTED_EDGE ( 'NONE', *, *, #1873, .F. ) ;
#11026 = PLANE ( 'NONE',  #2412 ) ;
#11027 = CARTESIAN_POINT ( 'NONE',  ( 51.84375000000001421, 8.757359312880723223, 18.00000000000000711 ) ) ;
#11028 = DIRECTION ( 'NONE',  ( -1.000000000000000000, 0.000000000000000000, 0.000000000000000000 ) ) ;
#11029 =( LENGTH_UNIT ( ) NAMED_UNIT ( * ) SI_UNIT ( .MILLI., .METRE. ) );
#11030 = ORIENTED_EDGE ( 'NONE', *, *, #23089, .F. ) ;
#11031 = DIRECTION ( 'NONE',  ( 0.000000000000000000, 0.000000000000000000, 1.000000000000000000 ) ) ;
#11032 = CARTESIAN_POINT ( 'NONE',  ( 3.458734125000000770, -1.432654583217639610, -0.8249999986344030978 ) ) ;
#11033 = CARTESIAN_POINT ( 'NONE',  ( -19.99999999999999645, -9.000000000000003553, 5.000000000000079936 ) ) ;
#11034 = ORIENTED_EDGE ( 'NONE', *, *, #20606, .T. ) ;
#11035 = CARTESIAN_POINT ( 'NONE',  ( 69.89999999999999147, 12.50000000000000000, 14.99999999999999645 ) ) ;
#11036 = ORIENTED_EDGE ( 'NONE', *, *, #19908, .T. ) ;
#11037 = CIRCLE ( 'NONE', #11419, 8.265000000000021885 ) ;
#11038 = LINE ( 'NONE', #7794, #6827 ) ;
#11039 = CARTESIAN_POINT ( 'NONE',  ( -3.999999999999998224, -1.656854249492383246, 19.06250000000001421 ) ) ;
#11040 = LINE ( 'NONE', #1553, #797 ) ;
#11041 = VECTOR ( 'NONE', #2198, 1000.000000000000114 ) ;
#11042 = VECTOR ( 'NONE', #9299, 1000.000000000000114 ) ;
#11043 = PLANE ( 'NONE',  #12999 ) ;
#11044 = ORIENTED_EDGE ( 'NONE', *, *, #19315, .F. ) ;
#11045 = CARTESIAN_POINT ( 'NONE',  ( -68.64999999999999147, 7.499999999999995559, 16.03553390593273420 ) ) ;
#11046 = ADVANCED_FACE ( 'NONE', ( #3807 ), #21880, .F. ) ;
#11047 = LINE ( 'NONE', #16903, #15297 ) ;
#11048 = EDGE_CURVE ( 'NONE', #6771, #14744, #7313, .T. ) ;
#11049 = CARTESIAN_POINT ( 'NONE',  ( 67.85000000109248219, 12.06698730000000097, 14.99999999999999645 ) ) ;
#11050 = CARTESIAN_POINT ( 'NONE',  ( 2.445694354108821855, -2.445694354108820079, 18.81250000136560629 ) ) ;
#11051 = DIRECTION ( 'NONE',  ( -1.000000000000000000, -0.000000000000000000, 0.000000000000000000 ) ) ;
#11052 = AXIS2_PLACEMENT_3D ( 'NONE', #4417, #19366, #2961 ) ;
#11053 = CARTESIAN_POINT ( 'NONE',  ( -1.432654583217641164, -3.458734125000000326, -2.824999998634404985 ) ) ;
#11054 = CARTESIAN_POINT ( 'NONE',  ( 68.20000000218495018, 9.999999999999998224, 12.49999999999999289 ) ) ;
#11055 = CARTESIAN_POINT ( 'NONE',  ( -3.458734124999998993, 1.432654583217640276, 15.37500000136560807 ) ) ;
#11056 = DIRECTION ( 'NONE',  ( -7.087422195345011518E-32, -1.000000000000000000, -0.000000000000000000 ) ) ;
#11057 = ORIENTED_EDGE ( 'NONE', *, *, #11465, .T. ) ;
#11058 = CIRCLE ( 'NONE', #15271, 6.500000000000000888 ) ;
#11059 = CARTESIAN_POINT ( 'NONE',  ( -69.50000000109247367, 12.06698729999999919, 15.85617417291294196 ) ) ;
#11060 = ORIENTED_EDGE ( 'NONE', *, *, #13054, .F. ) ;
#11061 = CARTESIAN_POINT ( 'NONE',  ( 56.12268183416157541, 12.78030770151606177, 17.87654654797631792 ) ) ;
#11062 = CARTESIAN_POINT ( 'NONE',  ( -70.50000000109245946, 12.06698730000000275, 15.85617417291294196 ) ) ;
#11063 = ITEM_DEFINED_TRANSFORMATION ( 'NONE', 'NONE', #9156,  #7318 ) ;
#11064 = AXIS2_PLACEMENT_3D ( 'NONE', #7681, #22249, #1781 ) ;
#11065 = CARTESIAN_POINT ( 'NONE',  ( 0.000000000000000000, -9.314797388894900720, 5.239665997526855357 ) ) ;
#11066 = ORIENTED_EDGE ( 'NONE', *, *, #15741, .T. ) ;
#11067 = ORIENTED_EDGE ( 'NONE', *, *, #21763, .T. ) ;
#11068 = CARTESIAN_POINT ( 'NONE',  ( 70.89999999999999147, 9.999999999999998224, 17.49999999999999645 ) ) ;
#11069 = AXIS2_PLACEMENT_3D ( 'NONE', #8277, #11997, #13795 ) ;
#11070 = CARTESIAN_POINT ( 'NONE',  ( 52.90856816583843880, 12.97181229448534978, 13.68930817193506755 ) ) ;
#11071 = AXIS2_PLACEMENT_3D ( 'NONE', #19668, #1111, #6758 ) ;
#11072 = CARTESIAN_POINT ( 'NONE',  ( -71.15000000109247935, 11.46158073645647235, 16.46158073645647235 ) ) ;
#11073 = CARTESIAN_POINT ( 'NONE',  ( -71.00000000109245946, 9.143825827087050939, 12.93301269999999370 ) ) ;
#11074 = CARTESIAN_POINT ( 'NONE',  ( -3.458734124999999437, 0.000000000000000000, 10.68750000136560452 ) ) ;
#11075 = CYLINDRICAL_SURFACE ( 'NONE', #18312, 4.000000000000001776 ) ;
#11076 = CARTESIAN_POINT ( 'NONE',  ( 52.21875000000002842, 13.00000000000000711, 16.24264068711927322 ) ) ;
#11077 = CARTESIAN_POINT ( 'NONE',  ( 0.000000000000000000, 0.000000000000000000, 2.039999999999998259 ) ) ;
#11078 = VECTOR ( 'NONE', #15095, 1000.000000000000000 ) ;
#11079 = CARTESIAN_POINT ( 'NONE',  ( 55.68750000000000000, 9.999999999999989342, 11.99999999999999467 ) ) ;
#11080 = CARTESIAN_POINT ( 'NONE',  ( -1.656854249492380138, -3.999999999999999112, 17.31250000273119483 ) ) ;
#11081 = AXIS2_PLACEMENT_3D ( 'NONE', #22013, #3831, #2017 ) ;
#11082 = LINE ( 'NONE', #16936, #8805 ) ;
#11083 = VECTOR ( 'NONE', #13410, 1000.000000000000000 ) ;
#11084 = ORIENTED_EDGE ( 'NONE', *, *, #23298, .F. ) ;
#11085 = CARTESIAN_POINT ( 'NONE',  ( 69.85000000218497007, 11.03553390593272177, 12.49999999999998046 ) ) ;
#11086 = CARTESIAN_POINT ( 'NONE',  ( 72.50000000000000000, 9.999999999999998224, 17.49999999999999645 ) ) ;
#11087 = ORIENTED_EDGE ( 'NONE', *, *, #17900, .T. ) ;
#11088 = CARTESIAN_POINT ( 'NONE',  ( 55.40625000000000000, 12.99999999999999645, 13.75735931288070191 ) ) ;
#11089 = CARTESIAN_POINT ( 'NONE',  ( -3.458734125000000326, 1.432654583217640276, 4.675000001365594571 ) ) ;
#11090 = PLANE ( 'NONE',  #4425 ) ;
#11091 = ORIENTED_EDGE ( 'NONE', *, *, #3345, .T. ) ;
#11092 = CARTESIAN_POINT ( 'NONE',  ( -20.00005079999999680, 5.400000000000000355, -1.000000000000000000 ) ) ;
#11093 = CARTESIAN_POINT ( 'NONE',  ( 4.000000000000001776, -1.656854249492379694, 17.43750000000001421 ) ) ;
#11094 = EDGE_CURVE ( 'NONE', #9522, #8785, #21125, .T. ) ;
#11095 = COLOUR_RGB ( '', 0.31764706, 0.68627451, 0.89019608) ;
#11096 = DIRECTION ( 'NONE',  ( 0.000000000000000000, 0.000000000000000000, 1.000000000000000000 ) ) ;
#11097 = AXIS2_PLACEMENT_3D ( 'NONE', #16243, #20039, #5566 ) ;
#11098 = CARTESIAN_POINT ( 'NONE',  ( -4.000000000000000000, 0.000000000000000000, -2.574999997268812457 ) ) ;
#11099 = EDGE_LOOP ( 'NONE', ( #5370, #20053, #3201, #167 ) ) ;
#11100 = LINE ( 'NONE', #1962, #3338 ) ;
#11101 = VECTOR ( 'NONE', #5509, 1000.000000000000000 ) ;
#11102 = EDGE_CURVE ( 'NONE', #14363, #20225, #3481, .T. ) ;
#11103 = CARTESIAN_POINT ( 'NONE',  ( -3.458734125000000770, 1.432654583217640498, -1.074999998634403431 ) ) ;
#11104 = AXIS2_PLACEMENT_3D ( 'NONE', #6415, #6294, #17436 ) ;
#11105 = CARTESIAN_POINT ( 'NONE',  ( 69.20000000000000284, 11.76776695296636888, 16.76776695296636532 ) ) ;
#11106 = CARTESIAN_POINT ( 'NONE',  ( 0.000000000000000000, 8.461683424509345741, -2.223716399045483350 ) ) ;
#11107 = AXIS2_PLACEMENT_3D ( 'NONE', #1513, #4875, #16263 ) ;
#11108 = CARTESIAN_POINT ( 'NONE',  ( -66.94999999999998863, 8.964466094067207180, 17.49999999999995026 ) ) ;
#11109 = CIRCLE ( 'NONE', #12264, 8.749000000000000554 ) ;
#11110 = CARTESIAN_POINT ( 'NONE',  ( 54.50231816583843170, 12.78030770151603868, 12.12345345202365188 ) ) ;
#11111 = CARTESIAN_POINT ( 'NONE',  ( 1.432654583217639832, 3.458734125000000326, 0.4250000013655961251 ) ) ;
#11112 = CARTESIAN_POINT ( 'NONE',  ( -3.458734124999999437, 1.432654583217640498, 14.62500000136560629 ) ) ;
#11113 = DIRECTION ( 'NONE',  ( 0.000000000000000000, 0.000000000000000000, 1.000000000000000000 ) ) ;
#11114 = DIRECTION ( 'NONE',  ( -1.000000000000000000, -0.000000000000000000, -0.000000000000000000 ) ) ;
#11115 = CARTESIAN_POINT ( 'NONE',  ( 36.99310306966726358, -11.25000000000000355, 10.00000000000008882 ) ) ;
#11116 = EDGE_LOOP ( 'NONE', ( #1538, #19253, #17279, #14840 ) ) ;
#11117 = FACE_OUTER_BOUND ( 'NONE', #20485, .T. ) ;
#11118 = CARTESIAN_POINT ( 'NONE',  ( 0.6507732100473444525, -4.243078065514795050, -0.2236248678334952777 ) ) ;
#11119 = DIRECTION ( 'NONE',  ( 0.000000000000000000, 0.000000000000000000, 1.000000000000000000 ) ) ;
#11120 = ORIENTED_EDGE ( 'NONE', *, *, #19407, .F. ) ;
#11121 = AXIS2_PLACEMENT_3D ( 'NONE', #20259, #7366, #5905 ) ;
#11122 = ORIENTED_EDGE ( 'NONE', *, *, #18466, .T. ) ;
#11123 = EDGE_CURVE ( 'NONE', #12919, #12610, #11255, .T. ) ;
#11124 = LINE ( 'NONE', #3666, #22068 ) ;
#11125 = ADVANCED_FACE ( 'NONE', ( #23578 ), #90, .F. ) ;
#11126 = EDGE_LOOP ( 'NONE', ( #19739, #10901, #2070, #1605 ) ) ;
#11127 = CARTESIAN_POINT ( 'NONE',  ( 54.65625000000000711, 6.000000000000004441, 16.65685424949239390 ) ) ;
#11128 = ORIENTED_EDGE ( 'NONE', *, *, #21666, .F. ) ;
#11129 = CARTESIAN_POINT ( 'NONE',  ( -16.41397198033274307, -11.25000000000000355, 5.000000000000079936 ) ) ;
#11130 = ORIENTED_EDGE ( 'NONE', *, *, #23395, .F. ) ;
#11131 = AXIS2_PLACEMENT_3D ( 'NONE', #2875, #2649, #8423 ) ;
#11132 = CARTESIAN_POINT ( 'NONE',  ( 54.68981816583844591, 9.931948859054346102, 10.99999999999999467 ) ) ;
#11133 = VECTOR ( 'NONE', #1684, 1000.000000000000114 ) ;
#11134 = EDGE_CURVE ( 'NONE', #10129, #8578, #19432, .T. ) ;
#11135 = CARTESIAN_POINT ( 'NONE',  ( 71.85000000109246798, 12.06698730000000097, 14.99999999999999645 ) ) ;
#11136 = CARTESIAN_POINT ( 'NONE',  ( 66.15000000000000568, 8.964466094067260471, 17.50000000000000355 ) ) ;
#11137 =( BOUNDED_CURVE ( )  B_SPLINE_CURVE ( 2, ( #725, #21065, #491, #7814, #17028, #2516, #11420, #15132, #6004 ),
 .UNSPECIFIED., .F., .F. ) 
 B_SPLINE_CURVE_WITH_KNOTS ( ( 3, 2, 2, 2, 3 ),
 ( 0.2999999999999999889, 0.3125000000000000000, 0.3250000000000000111, 0.3375000000000000222, 0.3499999999999999778 ),
 .UNSPECIFIED. ) 
 CURVE ( )  GEOMETRIC_REPRESENTATION_ITEM ( )  RATIONAL_B_SPLINE_CURVE ( ( 1.000000000000000000, 0.9238795325112867385, 1.000000000000000000, 0.9238795325112867385, 1.000000000000000000, 0.9238795325112867385, 1.000000000000000000, 0.9238795325112867385, 1.000000000000000000 ) ) 
 REPRESENTATION_ITEM ( '' )  );
#11138 = CARTESIAN_POINT ( 'NONE',  ( 72.15000000109246514, 11.46158073645647235, 16.46158073645647235 ) ) ;
#11139 = EDGE_LOOP ( 'NONE', ( #19480, #14324 ) ) ;
#11140 = CARTESIAN_POINT ( 'NONE',  ( -3.999999999999999112, 0.000000000000000000, 16.12500000273119838 ) ) ;
#11141 = CARTESIAN_POINT ( 'NONE',  ( -65.00000000000000000, 9.999999999999998224, 14.99999999999999645 ) ) ;
#11142 = CARTESIAN_POINT ( 'NONE',  ( 54.24768183416157541, 7.123453452023678523, 17.78030770151605822 ) ) ;
#11143 = LINE ( 'NONE', #20435, #19151 ) ;
#11144 = CARTESIAN_POINT ( 'NONE',  ( 0.000000000000000000, 0.000000000000000000, -0.3080913168122742518 ) ) ;
#11145 = AXIS2_PLACEMENT_3D ( 'NONE', #2566, #8696, #14328 ) ;
#11146 = CARTESIAN_POINT ( 'NONE',  ( -67.70000000000000284, 9.999999999999998224, 17.49999999999999645 ) ) ;
#11147 = CARTESIAN_POINT ( 'NONE',  ( 4.000000000000000888, 0.8228435280416209752, -3.430609588141487976 ) ) ;
#11148 = ORIENTED_EDGE ( 'NONE', *, *, #14362, .T. ) ;
#11149 = DIRECTION ( 'NONE',  ( -0.000000000000000000, -0.000000000000000000, -1.000000000000000000 ) ) ;
#11150 = CARTESIAN_POINT ( 'NONE',  ( -4.204114297095464359, 1.660363174096617156, -3.602136431857887011 ) ) ;
#11151 = EDGE_CURVE ( 'NONE', #4473, #19596, #12698, .T. ) ;
#11152 = FACE_OUTER_BOUND ( 'NONE', #3611, .T. ) ;
#11153 = SURFACE_SIDE_STYLE ('',( #2004 ) ) ;
#11154 = ORIENTED_EDGE ( 'NONE', *, *, #10860, .T. ) ;
#11155 = CARTESIAN_POINT ( 'NONE',  ( -3.999999999999999112, 1.539600717838996324, -3.300726591567078039 ) ) ;
#11156 = CARTESIAN_POINT ( 'NONE',  ( 4.999999999999999112, -9.314797388894900720, 5.239665997526855357 ) ) ;
#11157 = CARTESIAN_POINT ( 'NONE',  ( -90.00000000000000000, 0.000000000000000000, 0.000000000000000000 ) ) ;
#11158 = EDGE_CURVE ( 'NONE', #3223, #5947, #15446, .T. ) ;
#11159 = LINE ( 'NONE', #1578, #7585 ) ;
#11160 = ORIENTED_EDGE ( 'NONE', *, *, #22661, .T. ) ;
#11161 = DIRECTION ( 'NONE',  ( -0.000000000000000000, -0.000000000000000000, -1.000000000000000000 ) ) ;
#11162 = ORIENTED_EDGE ( 'NONE', *, *, #14055, .F. ) ;
#11163 = DIRECTION ( 'NONE',  ( 1.000000000000000000, 0.000000000000000000, 0.000000000000000000 ) ) ;
#11164 = CARTESIAN_POINT ( 'NONE',  ( 4.000000000000000888, 4.898587196589412829E-16, 16.50000000000001066 ) ) ;
#11165 = ADVANCED_FACE ( 'NONE', ( #15094 ), #22349, .T. ) ;
#11166 = DIRECTION ( 'NONE',  ( -0.000000000000000000, -0.000000000000000000, -1.000000000000000000 ) ) ;
#11167 = VECTOR ( 'NONE', #8281, 1000.000000000000000 ) ;
#11168 = EDGE_CURVE ( 'NONE', #12677, #14904, #8190, .T. ) ;
#11169 = FACE_OUTER_BOUND ( 'NONE', #10637, .T. ) ;
#11170 = CARTESIAN_POINT ( 'NONE',  ( -1.656854249492379472, 4.000000000000000000, 17.93750000273119483 ) ) ;
#11171 = PLANE ( 'NONE',  #11438 ) ;
#11172 = VERTEX_POINT ( 'NONE', #9581 ) ;
#11173 = CARTESIAN_POINT ( 'NONE',  ( 13.29415075323382034, -9.000000000000003553, 5.000000000000079936 ) ) ;
#11174 = LINE ( 'NONE', #13089, #1866 ) ;
#11175 = CARTESIAN_POINT ( 'NONE',  ( 72.25000000109247367, 9.999999999999998224, 17.06698730000000097 ) ) ;
#11176 = CARTESIAN_POINT ( 'NONE',  ( -2.445694354108819191, 2.445694354108820523, 17.31250000136560274 ) ) ;
#11177 = CARTESIAN_POINT ( 'NONE',  ( -5.560781378645575757, 6.809993116116508640E-16, -4.000000000000000000 ) ) ;
#11178 = LINE ( 'NONE', #7697, #15380 ) ;
#11179 = CARTESIAN_POINT ( 'NONE',  ( 4.000000000000000000, 4.898587196589412829E-16, 5.800000000000001599 ) ) ;
#11180 = DIRECTION ( 'NONE',  ( -1.000000000000000000, -7.703719777548943412E-32, 0.000000000000000000 ) ) ;
#11181 = CARTESIAN_POINT ( 'NONE',  ( 3.458734125000001214, 4.235727675282971730E-16, 11.93750000136560629 ) ) ;
#11182 = CARTESIAN_POINT ( 'NONE',  ( -67.25000000218494733, 7.499999999999996447, 13.96446609406725514 ) ) ;
#11183 = ORIENTED_EDGE ( 'NONE', *, *, #13944, .T. ) ;
#11184 = CARTESIAN_POINT ( 'NONE',  ( -70.35000000109248219, 11.46158073645647235, 16.46158073645647235 ) ) ;
#11185 = ORIENTED_EDGE ( 'NONE', *, *, #1665, .F. ) ;
#11186 = CARTESIAN_POINT ( 'NONE',  ( 54.81018183416157541, 14.00000000000000000, 15.06805114094561304 ) ) ;
#11187 = CARTESIAN_POINT ( 'NONE',  ( -69.70000000109246230, 12.06698730000000275, 15.85617417291294196 ) ) ;
#11188 = SHAPE_DEFINITION_REPRESENTATION ( #20982, #16640 ) ;
#11189 = FACE_OUTER_BOUND ( 'NONE', #21510, .T. ) ;
#11190 = ORIENTED_EDGE ( 'NONE', *, *, #4733, .F. ) ;
#11191 = ORIENTED_EDGE ( 'NONE', *, *, #8764, .F. ) ;
#11192 = CARTESIAN_POINT ( 'NONE',  ( -35.00000000000000711, 4.500000000000003553, 1.285879139104720791E-14 ) ) ;
#11193 = EDGE_CURVE ( 'NONE', #10807, #10456, #11618, .T. ) ;
#11194 = CARTESIAN_POINT ( 'NONE',  ( 54.75000000000000711, 7.878679656440361612, 17.12132034355964549 ) ) ;
#11195 = ADVANCED_FACE ( 'NONE', ( #4162 ), #675, .F. ) ;
#11196 = CARTESIAN_POINT ( 'NONE',  ( -71.75000000109248788, 11.46158073645647235, 13.53841926354352232 ) ) ;
#11197 = CARTESIAN_POINT ( 'NONE',  ( -71.45000000109247651, 9.999999999999998224, 17.06698730000000097 ) ) ;
#11198 = CARTESIAN_POINT ( 'NONE',  ( -2.445694354108818303, -2.445694354108820967, 10.81250000136560452 ) ) ;
#11199 = DIRECTION ( 'NONE',  ( 0.000000000000000000, 0.000000000000000000, -1.000000000000000000 ) ) ;
#11200 = CARTESIAN_POINT ( 'NONE',  ( 51.09375000000000000, 11.24264068711927322, 11.99999999999998934 ) ) ;
#11201 = DIRECTION ( 'NONE',  ( 0.000000000000000000, 0.000000000000000000, -1.000000000000000000 ) ) ;
#11202 = CARTESIAN_POINT ( 'NONE',  ( 51.00000000000000711, 12.12132034355963484, 12.87867965644034740 ) ) ;
#11203 = CARTESIAN_POINT ( 'NONE',  ( -3.999999999999999112, 0.000000000000000000, 14.12500000273119660 ) ) ;
#11204 = CARTESIAN_POINT ( 'NONE',  ( -69.20000000218495018, 12.50000000000000000, 14.99999999999999645 ) ) ;
#11205 = VERTEX_POINT ( 'NONE', #16874 ) ;
#11206 = CARTESIAN_POINT ( 'NONE',  ( 70.14999999999999147, 8.964466094067256918, 17.49999999999999289 ) ) ;
#11207 = CARTESIAN_POINT ( 'NONE',  ( -71.55000000218494449, 12.50000000000000000, 13.96446609406725692 ) ) ;
#11208 = ORIENTED_EDGE ( 'NONE', *, *, #9830, .F. ) ;
#11209 = CARTESIAN_POINT ( 'NONE',  ( 51.28125000000000000, 8.757359312880703683, 11.99999999999999822 ) ) ;
#11210 = CARTESIAN_POINT ( 'NONE',  ( 2.828427124746189847, 2.828427124746190291, -2.949999997268812901 ) ) ;
#11211 = AXIS2_PLACEMENT_3D ( 'NONE', #22242, #18426, #2003 ) ;
#11212 = DIRECTION ( 'NONE',  ( -1.000000000000000000, -0.000000000000000000, 0.000000000000000000 ) ) ;
#11213 = ORIENTED_EDGE ( 'NONE', *, *, #16815, .F. ) ;
#11214 = CARTESIAN_POINT ( 'NONE',  ( 1.656854249492381470, 4.000000000000000000, 17.68750000000001066 ) ) ;
#11215 = CYLINDRICAL_SURFACE ( 'NONE', #23636, 4.000000000000001776 ) ;
#11216 = PLANE ( 'NONE',  #8354 ) ;
#11217 = ORIENTED_EDGE ( 'NONE', *, *, #13381, .T. ) ;
#11218 = DIRECTION ( 'NONE',  ( -1.000000000000000000, -7.703719777548943412E-32, 0.000000000000000000 ) ) ;
#11219 = CARTESIAN_POINT ( 'NONE',  ( 1.432654583217640276, 3.458734125000000770, -0.3249999986344045411 ) ) ;
#11220 = CARTESIAN_POINT ( 'NONE',  ( 67.29999999999999716, 9.999999999999998224, 12.49999999999999289 ) ) ;
#11221 = AXIS2_PLACEMENT_3D ( 'NONE', #20351, #2396, #11292 ) ;
#11222 = LINE ( 'NONE', #4008, #7802 ) ;
#11223 = EDGE_CURVE ( 'NONE', #8640, #1126, #10055, .T. ) ;
#11224 = LINE ( 'NONE', #18498, #15323 ) ;
#11225 = CARTESIAN_POINT ( 'NONE',  ( 50.00231816583843170, 12.78030770151603868, 12.12345345202365188 ) ) ;
#11226 = CARTESIAN_POINT ( 'NONE',  ( -3.458734125000000326, 0.000000000000000000, -1.262499998634402765 ) ) ;
#11227 = CARTESIAN_POINT ( 'NONE',  ( 1.025207404391860050E-15, 3.458734125000000770, 15.43750000136560452 ) ) ;
#11228 = CARTESIAN_POINT ( 'NONE',  ( 68.90000000218495302, 8.232233047033629347, 13.23223304703362402 ) ) ;
#11229 = CARTESIAN_POINT ( 'NONE',  ( -71.25000000109247367, 12.06698730000000097, 14.99999999999999645 ) ) ;
#11230 = CARTESIAN_POINT ( 'NONE',  ( 44.00000000000000711, -9.796556200126378400, 10.00000000000008882 ) ) ;
#11231 = ORIENTED_EDGE ( 'NONE', *, *, #12812, .T. ) ;
#11232 = CARTESIAN_POINT ( 'NONE',  ( 19.99999999999999645, 1.500000000000003109, -50.00000000000000000 ) ) ;
#11233 = FACE_OUTER_BOUND ( 'NONE', #5652, .T. ) ;
#11234 = LINE ( 'NONE', #1630, #941 ) ;
#11235 = ORIENTED_EDGE ( 'NONE', *, *, #1873, .T. ) ;
#11236 = VERTEX_POINT ( 'NONE', #22601 ) ;
#11237 = CARTESIAN_POINT ( 'NONE',  ( 72.50000000000000000, 9.999999999999998224, 17.49999999999999645 ) ) ;
#11238 = CARTESIAN_POINT ( 'NONE',  ( 55.40625000000000711, 13.99999999999999289, 13.34314575050759544 ) ) ;
#11239 = ORIENTED_EDGE ( 'NONE', *, *, #6871, .F. ) ;
#11240 = CARTESIAN_POINT ( 'NONE',  ( 72.50000000000000000, 9.999999999999998224, 12.49999999999999289 ) ) ;
#11241 = ORIENTED_EDGE ( 'NONE', *, *, #137, .T. ) ;
#11242 = VECTOR ( 'NONE', #21001, 1000.000000000000000 ) ;
#11243 = CARTESIAN_POINT ( 'NONE',  ( 56.65856816583844591, 6.028187705514649330, 16.72490539043803182 ) ) ;
#11244 = AXIS2_PLACEMENT_3D ( 'NONE', #746, #20620, #2658 ) ;
#11245 = CARTESIAN_POINT ( 'NONE',  ( 66.00000000218494733, 12.50000000000000000, 14.99999999999999645 ) ) ;
#11246 = DIRECTION ( 'NONE',  ( -0.000000000000000000, -0.000000000000000000, -1.000000000000000000 ) ) ;
#11247 = CARTESIAN_POINT ( 'NONE',  ( 70.50000000109245946, 12.06698730000000275, 15.85617417291294196 ) ) ;
#11248 = PRODUCT ( 'spur gear_iso_ISO - Spur gear 1M 20T 20PA 5FW ---S20B12H25L8.0S1', 'spur gear_iso_ISO - Spur gear 1M 20T 20PA 5FW ---S20B12H25L8.0S1', '', ( #17032 ) ) ;
#11249 = ORIENTED_EDGE ( 'NONE', *, *, #7060, .F. ) ;
#11250 = CARTESIAN_POINT ( 'NONE',  ( -2.828427124746188515, -2.828427124746190735, 11.12500000000001066 ) ) ;
#11251 = ADVANCED_FACE ( 'NONE', ( #6443 ), #912, .T. ) ;
#11252 = LINE ( 'NONE', #4159, #13001 ) ;
#11253 = EDGE_CURVE ( 'NONE', #9804, #23245, #37, .T. ) ;
#11254 = CARTESIAN_POINT ( 'NONE',  ( 55.93518183416157541, 9.931948859054379852, 18.99999999999999289 ) ) ;
#11255 = LINE ( 'NONE', #5374, #14984 ) ;
#11256 = FACE_OUTER_BOUND ( 'NONE', #16667, .T. ) ;
#11257 = DIRECTION ( 'NONE',  ( -0.8191520442889875797, 1.003171929053519570E-16, 0.5735764363510522656 ) ) ;
#11258 = DIRECTION ( 'NONE',  ( 7.087422195345011518E-32, 1.000000000000000000, -0.000000000000000000 ) ) ;
#11259 = CARTESIAN_POINT ( 'NONE',  ( -3.250000000000004441, 5.629165124598849879, 0.000000000000000000 ) ) ;
#11260 = ORIENTED_EDGE ( 'NONE', *, *, #13054, .T. ) ;
#11261 = CARTESIAN_POINT ( 'NONE',  ( 1.799999999999996048, 0.000000000000000000, -9.000000000000023093 ) ) ;
#11262 = CARTESIAN_POINT ( 'NONE',  ( 4.999999999999999112, -4.057423117305329896, -8.475820894093020641 ) ) ;
#11263 = SURFACE_STYLE_USAGE ( .BOTH. , #11153 ) ;
#11264 = EDGE_CURVE ( 'NONE', #8578, #6397, #10902, .T. ) ;
#11265 = ORIENTED_EDGE ( 'NONE', *, *, #22086, .F. ) ;
#11266 = DIRECTION ( 'NONE',  ( 1.000000000000000000, -0.000000000000000000, -0.000000000000000000 ) ) ;
#11267 = CARTESIAN_POINT ( 'NONE',  ( 40.13469571966727045, -11.25000000000000355, 5.000000000000079936 ) ) ;
#11268 = PLANE ( 'NONE',  #18537 ) ;
#11269 = CARTESIAN_POINT ( 'NONE',  ( 2.828427124746192067, -2.828427124746189847, 16.50000000273119838 ) ) ;
#11270 = ORIENTED_EDGE ( 'NONE', *, *, #1910, .T. ) ;
#11271 = CARTESIAN_POINT ( 'NONE',  ( 2.344047193898588954, 3.265465875126468021, -5.031375706690542042E-16 ) ) ;
#11272 = ORIENTED_EDGE ( 'NONE', *, *, #14062, .T. ) ;
#11273 = DIRECTION ( 'NONE',  ( 0.000000000000000000, 0.000000000000000000, 1.000000000000000000 ) ) ;
#11274 =( BOUNDED_CURVE ( )  B_SPLINE_CURVE ( 2, ( #7550, #9010, #19982, #5747, #11035, #3585, #16302, #105, #14519 ),
 .UNSPECIFIED., .F., .F. ) 
 B_SPLINE_CURVE_WITH_KNOTS ( ( 3, 2, 2, 2, 3 ),
 ( 0.3749999999999998890, 0.3906249999999997780, 0.4062499999999996669, 0.4218749999999996114, 0.4374999999999995004 ),
 .UNSPECIFIED. ) 
 CURVE ( )  GEOMETRIC_REPRESENTATION_ITEM ( )  RATIONAL_B_SPLINE_CURVE ( ( 1.000000000000000444, 0.9238795325112861834, 1.000000000000000000, 0.9238795325112867385, 1.000000000000000000, 0.9238795325112867385, 1.000000000000000000, 0.9238795325112891810, 0.9999999999999975575 ) ) 
 REPRESENTATION_ITEM ( '' )  );
#11275 = CARTESIAN_POINT ( 'NONE',  ( 4.000000000000001776, -1.656854249492379694, 16.43750000000001066 ) ) ;
#11276 = CARTESIAN_POINT ( 'NONE',  ( 0.000000000000000000, 0.000000000000000000, -0.2800830152838844622 ) ) ;
#11277 = CYLINDRICAL_SURFACE ( 'NONE', #12641, 2.500000000000002220 ) ;
#11278 = FACE_OUTER_BOUND ( 'NONE', #1488, .T. ) ;
#11279 = CARTESIAN_POINT ( 'NONE',  ( 71.80000000109245661, 9.143825827087052716, 12.93301269999999192 ) ) ;
#11280 = VECTOR ( 'NONE', #2887, 1000.000000000000000 ) ;
#11281 = ORIENTED_EDGE ( 'NONE', *, *, #15949, .F. ) ;
#11282 = EDGE_CURVE ( 'NONE', #9434, #23552, #21158, .T. ) ;
#11283 = CYLINDRICAL_SURFACE ( 'NONE', #4153, 11.00000000000000000 ) ;
#11284 = EDGE_CURVE ( 'NONE', #14520, #12520, #7886, .T. ) ;
#11285 = VECTOR ( 'NONE', #2116, 1000.000000000000114 ) ;
#11286 = CARTESIAN_POINT ( 'NONE',  ( 7.347880794884118750E-16, -4.000000000000000000, -0.3249999972688121241 ) ) ;
#11287 = CARTESIAN_POINT ( 'NONE',  ( 67.10000000109248219, 12.06698730000000275, 15.85617417291294196 ) ) ;
#11288 = CARTESIAN_POINT ( 'NONE',  ( 2.445694354108821855, -2.445694354108820079, 16.81250000136560629 ) ) ;
#11289 = CARTESIAN_POINT ( 'NONE',  ( -19.99999999999999645, -15.00000000000001954, 5.000000000000079936 ) ) ;
#11290 = CARTESIAN_POINT ( 'NONE',  ( -3.458734125000000770, 0.000000000000000000, -3.012499998634404541 ) ) ;
#11291 = CARTESIAN_POINT ( 'NONE',  ( -1.656854249492381248, -3.999999999999999112, 5.487500000000000711 ) ) ;
#11292 = DIRECTION ( 'NONE',  ( 0.000000000000000000, 0.000000000000000000, 1.000000000000000000 ) ) ;
#11293 = CIRCLE ( 'NONE', #15128, 11.00000000000000000 ) ;
#11294 = CARTESIAN_POINT ( 'NONE',  ( 1.432654583217641164, 3.458734125000000326, 15.12500000136560807 ) ) ;
#11295 = DIRECTION ( 'NONE',  ( 1.000000000000000000, 0.000000000000000000, 0.000000000000000000 ) ) ;
#11296 = EDGE_CURVE ( 'NONE', #12123, #4946, #1554, .T. ) ;
#11297 = ADVANCED_FACE ( 'NONE', ( #6677 ), #19005, .F. ) ;
#11298 = VERTEX_POINT ( 'NONE', #3518 ) ;
#11299 = CARTESIAN_POINT ( 'NONE',  ( -67.85000000109248219, 12.06698730000000097, 14.99999999999999645 ) ) ;
#11300 = ORIENTED_EDGE ( 'NONE', *, *, #14342, .T. ) ;
#11301 = CARTESIAN_POINT ( 'NONE',  ( 51.99768183416157541, 12.87654654797631792, 12.21969229848393113 ) ) ;
#11302 = CARTESIAN_POINT ( 'NONE',  ( -69.35000000109246798, 8.538419263543524096, 13.53841926354352054 ) ) ;
#11303 = APPLICATION_PROTOCOL_DEFINITION ( 'draft international standard', 'automotive_design', 1998, #2570 ) ;
#11304 = ORIENTED_EDGE ( 'NONE', *, *, #21192, .T. ) ;
#11305 = CARTESIAN_POINT ( 'NONE',  ( -90.00000000000000000, 0.000000000000000000, 0.000000000000000000 ) ) ;
#11306 = VERTEX_POINT ( 'NONE', #12534 ) ;
#11307 = ORIENTED_EDGE ( 'NONE', *, *, #10206, .F. ) ;
#11308 = CARTESIAN_POINT ( 'NONE',  ( 1.872352939448454495E-15, -3.458734125000000770, 18.93750000136560629 ) ) ;
#11309 = CARTESIAN_POINT ( 'NONE',  ( 55.96875000000000000, 6.999999999999992895, 13.75735931288071967 ) ) ;
#11310 = CIRCLE ( 'NONE', #14368, 8.749000000000002331 ) ;
#11311 = VECTOR ( 'NONE', #7260, 1000.000000000000000 ) ;
#11312 = CARTESIAN_POINT ( 'NONE',  ( -68.30000000109247082, 7.933012699999995476, 14.14382582708705094 ) ) ;
#11313 = CIRCLE ( 'NONE', #16656, 6.735000000000022524 ) ;
#11314 = CARTESIAN_POINT ( 'NONE',  ( 68.45000000109247651, 9.999999999999998224, 12.93301269999999192 ) ) ;
#11315 = CARTESIAN_POINT ( 'NONE',  ( -68.60000000109246798, 9.143825827087050939, 12.93301269999999370 ) ) ;
#11316 = CARTESIAN_POINT ( 'NONE',  ( -3.458734124999999437, 1.432654583217640498, 12.62500000136560629 ) ) ;
#11317 = ADVANCED_FACE ( 'NONE', ( #9371 ), #16783, .F. ) ;
#11318 = FACE_OUTER_BOUND ( 'NONE', #19619, .T. ) ;
#11319 = CARTESIAN_POINT ( 'NONE',  ( 54.09375000000000711, 11.24264068711927322, 11.99999999999998934 ) ) ;
#11320 = CARTESIAN_POINT ( 'NONE',  ( 71.84999999999999432, 7.499999999999996447, 16.03553390593273775 ) ) ;
#11321 =( REPRESENTATION_RELATIONSHIP ('NONE','NONE', #8403, #10226 ) REPRESENTATION_RELATIONSHIP_WITH_TRANSFORMATION ( #6605 )SHAPE_REPRESENTATION_RELATIONSHIP( ) );
#11322 = EDGE_CURVE ( 'NONE', #2408, #15944, #16225, .T. ) ;
#11323 = CARTESIAN_POINT ( 'NONE',  ( 55.87500000000000711, 7.878679656440349177, 12.87867965644035984 ) ) ;
#11324 = CARTESIAN_POINT ( 'NONE',  ( 3.458734125000001214, 1.432654583217640498, 12.00000000136560807 ) ) ;
#11325 = CARTESIAN_POINT ( 'NONE',  ( 2.828427124746192067, -2.828427124746189847, 15.50000000273119660 ) ) ;
#11326 = LINE ( 'NONE', #16819, #11890 ) ;
#11327 = EDGE_CURVE ( 'NONE', #15248, #5525, #11178, .T. ) ;
#11328 = ORIENTED_EDGE ( 'NONE', *, *, #13379, .F. ) ;
#11329 = DIRECTION ( 'NONE',  ( 0.000000000000000000, 0.000000000000000000, -1.000000000000000000 ) ) ;
#11330 = DIRECTION ( 'NONE',  ( 0.9021819276640002938, 5.282584191382323161E-17, 0.4313557341643536880 ) ) ;
#11331 = ORIENTED_EDGE ( 'NONE', *, *, #10305, .F. ) ;
#11332 = CARTESIAN_POINT ( 'NONE',  ( 56.77893183416158251, 8.825410453826341595, 11.97181229448535511 ) ) ;
#11333 = AXIS2_PLACEMENT_3D ( 'NONE', #17034, #1076, #13568 ) ;
#11334 = CARTESIAN_POINT ( 'NONE',  ( 1.432654583217639832, 3.458734125000000326, 4.425000001365595459 ) ) ;
#11335 = AXIS2_PLACEMENT_3D ( 'NONE', #6207, #454, #18783 ) ;
#11336 = CARTESIAN_POINT ( 'NONE',  ( 34.67968829071656245, -8.974600000000002353, 5.000000000000079936 ) ) ;
#11337 = ORIENTED_EDGE ( 'NONE', *, *, #15139, .F. ) ;
#11338 = CARTESIAN_POINT ( 'NONE',  ( -3.999999999999999112, 0.000000000000000000, 15.00000000000001066 ) ) ;
#11339 = LINE ( 'NONE', #7615, #5292 ) ;
#11340 = DIRECTION ( 'NONE',  ( -0.000000000000000000, -0.000000000000000000, -1.000000000000000000 ) ) ;
#11341 = ORIENTED_EDGE ( 'NONE', *, *, #3688, .T. ) ;
#11342 = AXIS2_PLACEMENT_3D ( 'NONE', #19013, #11633, #9822 ) ;
#11343 = CIRCLE ( 'NONE', #1744, 6.500000000000000888 ) ;
#11344 = DIRECTION ( 'NONE',  ( -1.000000000000000000, -0.000000000000000000, -0.000000000000000000 ) ) ;
#11345 = CARTESIAN_POINT ( 'NONE',  ( -3.458734125000000770, 1.432654583217640498, 1.925000001365597457 ) ) ;
#11346 = CARTESIAN_POINT ( 'NONE',  ( 68.64999999999999147, 7.499999999999995559, 16.03553390593273420 ) ) ;
#11347 = CYLINDRICAL_SURFACE ( 'NONE', #16974, 2.500000000000002220 ) ;
#11348 = CARTESIAN_POINT ( 'NONE',  ( -0.6507732100473471171, 4.243078065514775510, -0.2236248678334823436 ) ) ;
#11349 = CARTESIAN_POINT ( 'NONE',  ( 58.34606816583844591, 8.825410453826357582, 18.02818770551464667 ) ) ;
#11350 = CARTESIAN_POINT ( 'NONE',  ( 3.458734125000000770, -1.432654583217639610, -2.824999998634404985 ) ) ;
#11351 = CARTESIAN_POINT ( 'NONE',  ( -1.432654583217639832, -3.458734125000000326, 13.87500000136560452 ) ) ;
#11352 = EDGE_CURVE ( 'NONE', #9624, #6314, #15014, .T. ) ;
#11353 = DIRECTION ( 'NONE',  ( 0.000000000000000000, 0.000000000000000000, -1.000000000000000000 ) ) ;
#11354 = FACE_OUTER_BOUND ( 'NONE', #12214, .T. ) ;
#11355 = EDGE_LOOP ( 'NONE', ( #18075, #20886, #18795, #5330, #5773, #6251 ) ) ;
#11356 = CARTESIAN_POINT ( 'NONE',  ( 2.499999999999999556, 9.915734732513218574, 4.762163868918309007 ) ) ;
#11357 = DIRECTION ( 'NONE',  ( -1.000000000000000000, -7.703719777548943412E-32, 0.000000000000000000 ) ) ;
#11358 = CARTESIAN_POINT ( 'NONE',  ( -71.25000000109248788, 9.999999999999998224, 17.06698730000000097 ) ) ;
#11359 = EDGE_LOOP ( 'NONE', ( #12694, #5707, #4385, #7868 ) ) ;
#11360 = ORIENTED_EDGE ( 'NONE', *, *, #9067, .F. ) ;
#11361 = DIRECTION ( 'NONE',  ( 1.060575238724910366E-16, -0.4999999999999951150, 0.8660254037844414832 ) ) ;
#11362 = CARTESIAN_POINT ( 'NONE',  ( 58.68750000000000000, 9.999999999999978684, 10.99999999999999645 ) ) ;
#11363 = ORIENTED_EDGE ( 'NONE', *, *, #19059, .F. ) ;
#11364 = CARTESIAN_POINT ( 'NONE',  ( 34.67044344676619971, -9.000000000000007105, 10.00000000000008882 ) ) ;
#11365 = VERTEX_POINT ( 'NONE', #18450 ) ;
#11366 = CARTESIAN_POINT ( 'NONE',  ( 54.50231816583843170, 12.78030770151603868, 12.12345345202365188 ) ) ;
#11367 = CARTESIAN_POINT ( 'NONE',  ( 65.65000000218493881, 7.499999999999995559, 13.96446609406725692 ) ) ;
#11368 = CARTESIAN_POINT ( 'NONE',  ( 9.920644283265380691E-16, 4.000000000000000000, 19.75000000000001066 ) ) ;
#11369 = CARTESIAN_POINT ( 'NONE',  ( 70.15000000109246514, 8.538419263543524096, 13.53841926354352054 ) ) ;
#11370 = VERTEX_POINT ( 'NONE', #11413 ) ;
#11371 = CARTESIAN_POINT ( 'NONE',  ( -3.999999999999999112, 0.000000000000000000, 14.12500000273119660 ) ) ;
#11372 = CARTESIAN_POINT ( 'NONE',  ( -4.000000000000000000, 0.000000000000000000, 0.4250000027311868211 ) ) ;
#11373 = CARTESIAN_POINT ( 'NONE',  ( 52.46643183416157541, 6.028187705514633343, 13.27509460956200016 ) ) ;
#11374 = CARTESIAN_POINT ( 'NONE',  ( 3.007318562400188799, 2.637429632093199139, 2.039999999999998259 ) ) ;
#11375 = PLANE ( 'NONE',  #18518 ) ;
#11376 = CARTESIAN_POINT ( 'NONE',  ( 50.00000000000000000, -10.00000000000001954, 15.00000000000002842 ) ) ;
#11377 = CARTESIAN_POINT ( 'NONE',  ( 0.000000000000000000, 0.000000000000000000, 0.000000000000000000 ) ) ;
#11378 = CARTESIAN_POINT ( 'NONE',  ( -1.065083781909173410, 6.890627091270371096, -0.2578475836320718306 ) ) ;
#11379 = ORIENTED_EDGE ( 'NONE', *, *, #19748, .F. ) ;
#11380 = CARTESIAN_POINT ( 'NONE',  ( 51.00000000000000711, 12.12132034355963484, 12.87867965644034740 ) ) ;
#11381 = CARTESIAN_POINT ( 'NONE',  ( 4.999999999999999112, -10.82112760146737784, 1.975651141462196669 ) ) ;
#11382 = FILL_AREA_STYLE_COLOUR ( '', #10388 ) ;
#11383 = VECTOR ( 'NONE', #3507, 1000.000000000000000 ) ;
#11384 = VERTEX_POINT ( 'NONE', #18922 ) ;
#11385 = CARTESIAN_POINT ( 'NONE',  ( 4.999999999999999112, -8.152713396088739017, -3.174628368996162298 ) ) ;
#11386 = CYLINDRICAL_SURFACE ( 'NONE', #20579, 2.500000000000000444 ) ;
#11387 = CARTESIAN_POINT ( 'NONE',  ( -1.301042606982605321E-15, 7.505553499465137612, -3.119443416399232394 ) ) ;
#11388 = CARTESIAN_POINT ( 'NONE',  ( 4.000000000000000888, 4.898587196589412829E-16, 11.50000000000001066 ) ) ;
#11389 = ORIENTED_EDGE ( 'NONE', *, *, #15921, .F. ) ;
#11390 = FACE_OUTER_BOUND ( 'NONE', #13248, .T. ) ;
#11391 = ORIENTED_EDGE ( 'NONE', *, *, #1665, .T. ) ;
#11392 = ORIENTED_EDGE ( 'NONE', *, *, #4796, .T. ) ;
#11393 = ADVANCED_FACE ( 'NONE', ( #20711 ), #15718, .T. ) ;
#11394 = DIRECTION ( 'NONE',  ( -1.000000000000000000, -7.703719777548943412E-32, 0.000000000000000000 ) ) ;
#11395 = VECTOR ( 'NONE', #14211, 1000.000000000000000 ) ;
#11396 = CARTESIAN_POINT ( 'NONE',  ( 1.971781867644420635E-15, -4.000000000000000000, 13.25000000000001243 ) ) ;
#11397 = DIRECTION ( 'NONE',  ( -0.9396926207859107594, -0.3420201433256623291, 1.540743955509804830E-32 ) ) ;
#11398 = CIRCLE ( 'NONE', #4104, 4.000000000000000000 ) ;
#11399 = DIRECTION ( 'NONE',  ( -0.000000000000000000, -0.000000000000000000, 1.000000000000000000 ) ) ;
#11400 = DIRECTION ( 'NONE',  ( 1.000000000000000000, -0.000000000000000000, -0.000000000000000000 ) ) ;
#11401 = CARTESIAN_POINT ( 'NONE',  ( 71.90000000109246514, 10.85617417291294551, 12.93301269999999192 ) ) ;
#11402 = ADVANCED_FACE ( 'NONE', ( #15597 ), #832, .T. ) ;
#11403 = VERTEX_POINT ( 'NONE', #10086 ) ;
#11404 = AXIS2_PLACEMENT_3D ( 'NONE', #19954, #23321, #7165 ) ;
#11405 = VECTOR ( 'NONE', #9351, 1000.000000000000114 ) ;
#11406 = DIRECTION ( 'NONE',  ( 1.224646799147353207E-16, 0.000000000000000000, 1.000000000000000000 ) ) ;
#11407 = DIRECTION ( 'NONE',  ( 1.000000000000000000, 0.000000000000000000, 0.000000000000000000 ) ) ;
#11408 = CARTESIAN_POINT ( 'NONE',  ( 67.95000000109247651, 11.46158073645647235, 16.46158073645647235 ) ) ;
#11409 = CARTESIAN_POINT ( 'NONE',  ( 3.458734125000001214, 4.235727675282971730E-16, 16.93750000136560629 ) ) ;
#11410 = B_SPLINE_CURVE_WITH_KNOTS ( 'NONE', 3,
 ( #1424, #5042, #12373, #7084, #2, #7333, #19637, #3356 ),
 .UNSPECIFIED., .F., .F.,
 ( 4, 2, 2, 4 ),
 ( 0.005725059856848641743, 0.006314084072593626612, 0.006903108288338611481, 0.008081156719828581220 ),
 .UNSPECIFIED. ) ;
#11411 = DIRECTION ( 'NONE',  ( 0.9396926207859107594, -0.3420201433256623291, 3.697785493223492838E-32 ) ) ;
#11412 = AXIS2_PLACEMENT_3D ( 'NONE', #7123, #10386, #12169 ) ;
#11413 = CARTESIAN_POINT ( 'NONE',  ( 15.82088754676620823, -9.000000000000005329, 5.000000000000079936 ) ) ;
#11414 = CARTESIAN_POINT ( 'NONE',  ( -2.828427124746190291, 2.828427124746190291, 2.175000000000001599 ) ) ;
#11415 = DIRECTION ( 'NONE',  ( 0.000000000000000000, 0.000000000000000000, -1.000000000000000000 ) ) ;
#11416 = CARTESIAN_POINT ( 'NONE',  ( 2.445694354108821855, -2.445694354108820079, 12.81250000136560629 ) ) ;
#11417 = DIRECTION ( 'NONE',  ( -1.000000000000000000, 0.000000000000000000, 0.000000000000000000 ) ) ;
#11418 = ORIENTED_EDGE ( 'NONE', *, *, #2604, .T. ) ;
#11419 = AXIS2_PLACEMENT_3D ( 'NONE', #2737, #11993, #17486 ) ;
#11420 = CARTESIAN_POINT ( 'NONE',  ( 2.828427124746191179, 2.828427124746190291, 15.75000000273119660 ) ) ;
#11421 = EDGE_LOOP ( 'NONE', ( #10693, #17681, #22722, #16271 ) ) ;
#11422 = CARTESIAN_POINT ( 'NONE',  ( 56.43750000000000000, 10.00000000000001776, 18.99999999999999645 ) ) ;
#11423 = CARTESIAN_POINT ( 'NONE',  ( -70.85000000109246798, 7.933012699999995476, 14.99999999999999645 ) ) ;
#11424 = CONTEXT_DEPENDENT_SHAPE_REPRESENTATION ( #261, #5682 ) ;
#11425 =( BOUNDED_CURVE ( )  B_SPLINE_CURVE ( 2, ( #19141, #8025, #22728, #5977, #10188, #22845, #11635, #6095, #2605 ),
 .UNSPECIFIED., .F., .F. ) 
 B_SPLINE_CURVE_WITH_KNOTS ( ( 3, 2, 2, 2, 3 ),
 ( 0.1249999999999992367, 0.1406249999999996947, 0.1562500000000001388, 0.1718750000000005829, 0.1875000000000010270 ),
 .UNSPECIFIED. ) 
 CURVE ( )  GEOMETRIC_REPRESENTATION_ITEM ( )  RATIONAL_B_SPLINE_CURVE ( ( 1.000000000000003775, 0.9238795325112830747, 1.000000000000000000, 0.9238795325112867385, 1.000000000000000000, 0.9238795325112867385, 1.000000000000000000, 0.9238795325112817425, 1.000000000000005107 ) ) 
 REPRESENTATION_ITEM ( '' )  );
#11426 = EDGE_LOOP ( 'NONE', ( #3320, #4204, #4394, #10545 ) ) ;
#11427 = DIRECTION ( 'NONE',  ( -1.000000000000000000, -0.000000000000000000, -0.000000000000000000 ) ) ;
#11428 = ORIENTED_EDGE ( 'NONE', *, *, #4034, .F. ) ;
#11429 = AXIS2_PLACEMENT_3D ( 'NONE', #2930, #10403, #10517 ) ;
#11430 = EDGE_CURVE ( 'NONE', #7815, #19956, #4315, .T. ) ;
#11431 = EDGE_CURVE ( 'NONE', #19924, #15228, #13833, .T. ) ;
#11432 = ORIENTED_EDGE ( 'NONE', *, *, #22260, .F. ) ;
#11433 = CARTESIAN_POINT ( 'NONE',  ( -3.458734124999998993, -1.432654583217642497, 18.75000000136560274 ) ) ;
#11434 = CARTESIAN_POINT ( 'NONE',  ( 58.03125000000000711, 11.24264068711929276, 18.00000000000000355 ) ) ;
#11435 = CARTESIAN_POINT ( 'NONE',  ( -66.85000000109248219, 9.999999999999998224, 12.93301269999999192 ) ) ;
#11436 = CARTESIAN_POINT ( 'NONE',  ( 68.15000000109247935, 8.538419263543522320, 16.46158073645647235 ) ) ;
#11437 = EDGE_CURVE ( 'NONE', #844, #15758, #3856, .T. ) ;
#11438 = AXIS2_PLACEMENT_3D ( 'NONE', #23364, #9016, #9254 ) ;
#11439 = CARTESIAN_POINT ( 'NONE',  ( -67.15000000109247935, 11.46158073645647235, 13.53841926354352232 ) ) ;
#11440 = DIRECTION ( 'NONE',  ( 0.000000000000000000, 0.000000000000000000, 1.000000000000000000 ) ) ;
#11441 = CARTESIAN_POINT ( 'NONE',  ( 56.77893183416158251, 8.825410453826341595, 11.97181229448535511 ) ) ;
#11442 = DIRECTION ( 'NONE',  ( -0.8660254037844373753, 0.5000000000000021094, 0.000000000000000000 ) ) ;
#11443 = AXIS2_PLACEMENT_3D ( 'NONE', #20980, #19549, #3264 ) ;
#11444 = AXIS2_PLACEMENT_3D ( 'NONE', #1778, #9122, #16411 ) ;
#11445 = CARTESIAN_POINT ( 'NONE',  ( 2.445694354108820079, 2.445694354108820523, 5.612500001365596347 ) ) ;
#11446 = CARTESIAN_POINT ( 'NONE',  ( -3.458734124999998105, 1.432654583217640276, 11.37500000136560452 ) ) ;
#11447 = CARTESIAN_POINT ( 'NONE',  ( 1.656854249492384135, -3.999999999999999112, 14.43750000273119483 ) ) ;
#11448 = CARTESIAN_POINT ( 'NONE',  ( 4.000000000000000000, 2.309401076758497151, -3.433295621305379353 ) ) ;
#11449 = VERTEX_POINT ( 'NONE', #12117 ) ;
#11450 = CARTESIAN_POINT ( 'NONE',  ( 2.500000000000000000, 2.357898499370431722, -2.818925648462311528E-15 ) ) ;
#11451 = ORIENTED_EDGE ( 'NONE', *, *, #21323, .T. ) ;
#11452 = CARTESIAN_POINT ( 'NONE',  ( 57.90393183416158251, 13.02818770551463778, 13.82541045382633982 ) ) ;
#11453 = CARTESIAN_POINT ( 'NONE',  ( -2.445694354108820523, 2.445694354108820523, 3.612500001365594571 ) ) ;
#11454 = EDGE_CURVE ( 'NONE', #1550, #21989, #2627, .T. ) ;
#11455 = CARTESIAN_POINT ( 'NONE',  ( 4.000000000000000000, 1.656854249492381248, 1.862500000000001599 ) ) ;
#11456 = ORIENTED_EDGE ( 'NONE', *, *, #2644, .T. ) ;
#11457 = CARTESIAN_POINT ( 'NONE',  ( -1.656854249492380138, -3.999999999999999112, 14.18750000000001066 ) ) ;
#11458 = VECTOR ( 'NONE', #9718, 1000.000000000000000 ) ;
#11459 = DIRECTION ( 'NONE',  ( 0.000000000000000000, 0.000000000000000000, 1.000000000000000000 ) ) ;
#11460 = EDGE_CURVE ( 'NONE', #9455, #5926, #21439, .T. ) ;
#11461 = LINE ( 'NONE', #18610, #21314 ) ;
#11462 = EDGE_LOOP ( 'NONE', ( #874, #13506, #18903, #18538 ) ) ;
#11463 = CARTESIAN_POINT ( 'NONE',  ( -71.40000000218495302, 9.999999999999998224, 12.49999999999999289 ) ) ;
#11464 = AXIS2_PLACEMENT_3D ( 'NONE', #2101, #22095, #18407 ) ;
#11465 = EDGE_CURVE ( 'NONE', #10566, #6989, #20281, .T. ) ;
#11466 = CARTESIAN_POINT ( 'NONE',  ( -1.432654583217641164, -3.458734125000000326, -0.8249999986344029868 ) ) ;
#11467 = ADVANCED_FACE ( 'NONE', ( #17021, #20936 ), #19037, .T. ) ;
#11468 = CARTESIAN_POINT ( 'NONE',  ( -4.000000000000000888, -2.309401076758512694, -3.504269196027526512 ) ) ;
#11469 = CARTESIAN_POINT ( 'NONE',  ( 69.09999999999999432, 12.50000000000000000, 14.99999999999999645 ) ) ;
#11470 = VECTOR ( 'NONE', #3839, 1000.000000000000000 ) ;
#11471 = DIRECTION ( 'NONE',  ( 1.000000000000000000, 0.000000000000000000, 0.000000000000000000 ) ) ;
#11472 = VECTOR ( 'NONE', #19502, 1000.000000000000000 ) ;
#11473 = CARTESIAN_POINT ( 'NONE',  ( -67.29999999999999716, 9.999999999999998224, 12.49999999999999289 ) ) ;
#11474 = CARTESIAN_POINT ( 'NONE',  ( 54.78356816583844591, 8.275094609561968184, 11.02818770551464667 ) ) ;
#11475 = CARTESIAN_POINT ( 'NONE',  ( 2.445694354108820523, -2.445694354108820079, -2.887499998634404097 ) ) ;
#11476 = CARTESIAN_POINT ( 'NONE',  ( -1.432654583217639832, -3.458734125000000326, 15.87500000136560807 ) ) ;
#11477 =( NAMED_UNIT ( * ) SI_UNIT ( $, .STERADIAN. ) SOLID_ANGLE_UNIT ( ) );
#11478 = CARTESIAN_POINT ( 'NONE',  ( -70.45000000109247651, 12.06698730000000097, 14.99999999999999645 ) ) ;
#11479 = ORIENTED_EDGE ( 'NONE', *, *, #5657, .T. ) ;
#11480 = CARTESIAN_POINT ( 'NONE',  ( 4.000000000000000888, 1.656854249492381248, 16.56250000000001066 ) ) ;
#11481 = ORIENTED_EDGE ( 'NONE', *, *, #19514, .F. ) ;
#11482 = CARTESIAN_POINT ( 'NONE',  ( 0.1404048886732821022, 4.699864953788070565, -3.686887068327037387 ) ) ;
#11483 = COLOUR_RGB ( '', 0.09019608, 0.27058824, 0.51372549) ;
#11484 = DIRECTION ( 'NONE',  ( 1.000000000000000000, -0.000000000000000000, -0.000000000000000000 ) ) ;
#11485 = CARTESIAN_POINT ( 'NONE',  ( -71.80000000109247082, 12.06698730000000275, 14.14382582708705094 ) ) ;
#11486 = VERTEX_POINT ( 'NONE', #19268 ) ;
#11487 = EDGE_LOOP ( 'NONE', ( #3318, #3813, #18171 ) ) ;
#11488 = DIRECTION ( 'NONE',  ( -1.000000000000000000, 0.000000000000000000, 0.000000000000000000 ) ) ;
#11489 = B_SPLINE_CURVE_WITH_KNOTS ( 'NONE', 3,
 ( #3691, #11155, #14865, #2007, #5500 ),
 .UNSPECIFIED., .F., .F.,
 ( 4, 1, 4 ),
 ( 0.000000000000000000, 0.002309401076758505790, 0.004618802153517011580 ),
 .UNSPECIFIED. ) ;
#11490 = VECTOR ( 'NONE', #12961, 1000.000000000000114 ) ;
#11491 = DIRECTION ( 'NONE',  ( 0.3420201433256622181, -0.9396926207859107594, 0.000000000000000000 ) ) ;
#11492 = VERTEX_POINT ( 'NONE', #6594 ) ;
#11493 = LINE ( 'NONE', #18766, #22132 ) ;
#11494 = ORIENTED_EDGE ( 'NONE', *, *, #19315, .T. ) ;
#11495 = AXIS2_PLACEMENT_3D ( 'NONE', #17694, #10290, #15901 ) ;
#11496 = UNCERTAINTY_MEASURE_WITH_UNIT (LENGTH_MEASURE( 1.000000000000000082E-05 ), #16970, 'distance_accuracy_value', 'NONE');
#11497 = CARTESIAN_POINT ( 'NONE',  ( 53.65856816583844591, 6.028187705514649330, 16.72490539043803182 ) ) ;
#11498 = ADVANCED_FACE ( 'NONE', ( #17264 ), #6479, .T. ) ;
#11499 = CARTESIAN_POINT ( 'NONE',  ( 70.15000000109247935, 11.46158073645647235, 13.53841926354352232 ) ) ;
#11500 = EDGE_CURVE ( 'NONE', #23556, #5711, #22509, .T. ) ;
#11501 = CARTESIAN_POINT ( 'NONE',  ( 2.828427124746191179, 2.828427124746190291, 19.62500000000001066 ) ) ;
#11502 = VECTOR ( 'NONE', #13858, 1000.000000000000000 ) ;
#11503 = CARTESIAN_POINT ( 'NONE',  ( 70.30000000109248504, 10.85617417291294551, 12.93301269999999370 ) ) ;
#11504 = ORIENTED_EDGE ( 'NONE', *, *, #15603, .F. ) ;
#11505 = CARTESIAN_POINT ( 'NONE',  ( 4.000000000000000888, 4.898587196589412829E-16, 12.62500000273119660 ) ) ;
#11506 = FACE_OUTER_BOUND ( 'NONE', #22638, .T. ) ;
#11507 = CARTESIAN_POINT ( 'NONE',  ( 55.56018183416157541, 5.999999999999996447, 14.93194885905437808 ) ) ;
#11508 = CARTESIAN_POINT ( 'NONE',  ( -2.149474931388143606, -6.264553569211847694, -3.644669744206375572 ) ) ;
#11509 = CARTESIAN_POINT ( 'NONE',  ( 45.00000000000000000, -10.00000000000001954, 12.50000000000002665 ) ) ;
#11510 = AXIS2_PLACEMENT_3D ( 'NONE', #21934, #9512, #12874 ) ;
#11511 = DIRECTION ( 'NONE',  ( 0.000000000000000000, 0.000000000000000000, -1.000000000000000000 ) ) ;
#11512 = CARTESIAN_POINT ( 'NONE',  ( -67.30000000109247082, 12.06698729999999919, 15.85617417291294196 ) ) ;
#11513 = DIRECTION ( 'NONE',  ( -0.000000000000000000, -1.000000000000000000, -0.000000000000000000 ) ) ;
#11514 = ORIENTED_EDGE ( 'NONE', *, *, #903, .F. ) ;
#11515 = CARTESIAN_POINT ( 'NONE',  ( 4.000000000000000888, 4.898587196589412829E-16, 12.50000000000001066 ) ) ;
#11516 = DIRECTION ( 'NONE',  ( 0.000000000000000000, 0.000000000000000000, 1.000000000000000000 ) ) ;
#11517 = VECTOR ( 'NONE', #14598, 1000.000000000000000 ) ;
#11518 = ORIENTED_EDGE ( 'NONE', *, *, #18003, .F. ) ;
#11519 = CARTESIAN_POINT ( 'NONE',  ( 4.999999999999999112, 0.000000000000000000, 0.000000000000000000 ) ) ;
#11520 = DIRECTION ( 'NONE',  ( 0.3420201433256622181, 0.9396926207859107594, -6.162975822039141593E-32 ) ) ;
#11521 = CARTESIAN_POINT ( 'NONE',  ( 4.000000000000000888, 4.898587196589412829E-16, 11.62500000273119660 ) ) ;
#11522 = AXIS2_PLACEMENT_3D ( 'NONE', #2283, #13327, #12855 ) ;
#11523 = DIRECTION ( 'NONE',  ( 0.000000000000000000, 0.000000000000000000, -1.000000000000000000 ) ) ;
#11524 = ORIENTED_EDGE ( 'NONE', *, *, #11322, .F. ) ;
#11525 = DIRECTION ( 'NONE',  ( -1.000000000000000000, -0.000000000000000000, -0.000000000000000000 ) ) ;
#11526 = ORIENTED_EDGE ( 'NONE', *, *, #16449, .F. ) ;
#11527 = DIRECTION ( 'NONE',  ( 0.000000000000000000, 0.000000000000000000, -1.000000000000000000 ) ) ;
#11528 = CARTESIAN_POINT ( 'NONE',  ( -3.999999999999999112, 0.000000000000000000, 16.00000000000001066 ) ) ;
#11529 = CARTESIAN_POINT ( 'NONE',  ( 4.999999999999999112, -8.264486777890139635, 4.472189673936757259 ) ) ;
#11530 = CARTESIAN_POINT ( 'NONE',  ( -65.00000000000000000, -10.00000000000000178, 14.99999999999999467 ) ) ;
#11531 = FACE_OUTER_BOUND ( 'NONE', #20333, .T. ) ;
#11532 = CARTESIAN_POINT ( 'NONE',  ( 71.35000000109246798, 11.46158073645647235, 16.46158073645647235 ) ) ;
#11533 = ORIENTED_EDGE ( 'NONE', *, *, #5457, .T. ) ;
#11534 = VECTOR ( 'NONE', #17678, 1000.000000000000000 ) ;
#11535 = CARTESIAN_POINT ( 'NONE',  ( 0.000000000000000000, -10.82112760146734765, -1.975651141462352767 ) ) ;
#11536 = CYLINDRICAL_SURFACE ( 'NONE', #5317, 4.000000000000000000 ) ;
#11537 = CARTESIAN_POINT ( 'NONE',  ( 67.60000000109248219, 9.143825827087050939, 12.93301269999999370 ) ) ;
#11538 = CARTESIAN_POINT ( 'NONE',  ( 1.432654583217643163, -3.458734124999999437, 14.75000000136560452 ) ) ;
#11539 = CARTESIAN_POINT ( 'NONE',  ( 37.81203609676620658, -9.000000000000005329, 5.000000000000079936 ) ) ;
#11540 = ADVANCED_FACE ( 'NONE', ( #13556 ), #9971, .F. ) ;
#11541 = CARTESIAN_POINT ( 'NONE',  ( -1.432654583217640498, 3.458734125000000770, -2.199999998634404541 ) ) ;
#11542 = CARTESIAN_POINT ( 'NONE',  ( 2.828427124746189847, 2.828427124746190291, -0.07499999999999867883 ) ) ;
#11543 = LINE ( 'NONE', #18812, #14785 ) ;
#11544 = CARTESIAN_POINT ( 'NONE',  ( -20.00005079999999680, 3.872983346207417021, 1.000000000000000000 ) ) ;
#11545 = FACE_OUTER_BOUND ( 'NONE', #8823, .T. ) ;
#11546 = EDGE_LOOP ( 'NONE', ( #1571, #22972, #10448, #688 ) ) ;
#11547 = CARTESIAN_POINT ( 'NONE',  ( -66.90000000109247935, 10.85617417291294551, 12.93301269999999192 ) ) ;
#11548 = EDGE_LOOP ( 'NONE', ( #8343, #10310, #8063, #11776 ) ) ;
#11549 = CARTESIAN_POINT ( 'NONE',  ( 60.00000000000000711, 12.82842712474617741, 12.17157287525379239 ) ) ;
#11550 = CARTESIAN_POINT ( 'NONE',  ( -70.45000000109247651, 12.06698730000000097, 14.99999999999999645 ) ) ;
#11551 = ORIENTED_EDGE ( 'NONE', *, *, #9977, .T. ) ;
#11552 = CARTESIAN_POINT ( 'NONE',  ( -69.29999999999999716, 9.999999999999998224, 17.49999999999999645 ) ) ;
#11553 = VERTEX_POINT ( 'NONE', #4553 ) ;
#11554 = AXIS2_PLACEMENT_3D ( 'NONE', #15205, #4284, #4515 ) ;
#11555 = ORIENTED_EDGE ( 'NONE', *, *, #17291, .T. ) ;
#11556 = CARTESIAN_POINT ( 'NONE',  ( -1.432654583217639832, -3.458734125000000326, 15.87500000136560807 ) ) ;
#11557 = CARTESIAN_POINT ( 'NONE',  ( 54.93750000000000711, 10.00000000000000711, 17.99999999999999645 ) ) ;
#11558 = CARTESIAN_POINT ( 'NONE',  ( -67.15000000109247935, 11.46158073645647235, 16.46158073645647235 ) ) ;
#11559 = CARTESIAN_POINT ( 'NONE',  ( 67.70000000109247651, 10.85617417291294551, 12.93301269999999192 ) ) ;
#11560 = CARTESIAN_POINT ( 'NONE',  ( -72.25000000000000000, 12.50000000000000000, 13.96446609406725869 ) ) ;
#11561 = PLANE ( 'NONE',  #4924 ) ;
#11562 = CARTESIAN_POINT ( 'NONE',  ( 54.52893183416158962, 11.17458954617365663, 18.02818770551464311 ) ) ;
#11563 = FACE_OUTER_BOUND ( 'NONE', #11359, .T. ) ;
#11564 = EDGE_CURVE ( 'NONE', #23470, #17148, #16876, .T. ) ;
#11565 =( BOUNDED_CURVE ( )  B_SPLINE_CURVE ( 2, ( #16543, #1793, #14764, #7565, #11286, #7342, #12741, #16657, #22018 ),
 .UNSPECIFIED., .F., .F. ) 
 B_SPLINE_CURVE_WITH_KNOTS ( ( 3, 2, 2, 2, 3 ),
 ( 0.5500000000000000444, 0.5625000000000000000, 0.5749999999999999556, 0.5875000000000000222, 0.5999999999999999778 ),
 .UNSPECIFIED. ) 
 CURVE ( )  GEOMETRIC_REPRESENTATION_ITEM ( )  RATIONAL_B_SPLINE_CURVE ( ( 1.000000000000000000, 0.9238795325112867385, 1.000000000000000000, 0.9238795325112867385, 1.000000000000000000, 0.9238795325112867385, 1.000000000000000000, 0.9238795325112867385, 1.000000000000000000 ) ) 
 REPRESENTATION_ITEM ( '' )  );
#11566 = CARTESIAN_POINT ( 'NONE',  ( 1.432654583217642275, -3.458734124999999882, 4.300000001365595459 ) ) ;
#11567 = EDGE_CURVE ( 'NONE', #6908, #7519, #945, .T. ) ;
#11568 = CARTESIAN_POINT ( 'NONE',  ( 1.432654583217641164, 3.458734125000000326, 11.12500000136560452 ) ) ;
#11569 = CARTESIAN_POINT ( 'NONE',  ( -3.999999999999999112, 1.656854249492380804, 14.06250000273119660 ) ) ;
#11570 = CARTESIAN_POINT ( 'NONE',  ( 4.999999999999999112, -1.975651141462315907, 10.82112760146735475 ) ) ;
#11571 = ORIENTED_EDGE ( 'NONE', *, *, #20871, .T. ) ;
#11572 = CARTESIAN_POINT ( 'NONE',  ( 45.00000000000000000, -10.00000000000001599, 34.11836509645782201 ) ) ;
#11573 = ORIENTED_EDGE ( 'NONE', *, *, #3652, .T. ) ;
#11574 = CARTESIAN_POINT ( 'NONE',  ( 60.34143183416158962, 8.689308171935088865, 17.97181229448535689 ) ) ;
#11575 = CARTESIAN_POINT ( 'NONE',  ( 1.432654583217642275, -3.458734124999999437, 3.050000001365598568 ) ) ;
#11576 = ADVANCED_FACE ( 'NONE', ( #21056 ), #6557, .T. ) ;
#11577 = CARTESIAN_POINT ( 'NONE',  ( 25.00005080000000035, 4.898587196589412829E-16, -4.000000000000000000 ) ) ;
#11578 = ORIENTED_EDGE ( 'NONE', *, *, #17427, .T. ) ;
#11579 = CARTESIAN_POINT ( 'NONE',  ( -3.999999999999999112, 0.000000000000000000, 14.00000000000001066 ) ) ;
#11580 = DIRECTION ( 'NONE',  ( -1.000000000000000000, -0.000000000000000000, -0.000000000000000000 ) ) ;
#11581 = DIRECTION ( 'NONE',  ( 0.5000000000000013323, 0.000000000000000000, 0.8660254037844380415 ) ) ;
#11582 = EDGE_LOOP ( 'NONE', ( #6371, #21628, #19818, #23675 ) ) ;
#11583 = CARTESIAN_POINT ( 'NONE',  ( -69.30000000218494449, 11.76776695296636888, 16.76776695296636532 ) ) ;
#11584 = CARTESIAN_POINT ( 'NONE',  ( 2.445694354108820967, -2.445694354108820079, -1.637499998634403209 ) ) ;
#11585 = B_SPLINE_CURVE_WITH_KNOTS ( 'NONE', 3,
 ( #12502, #21547, #12261, #23600, #10589, #21429, #21304, #15951 ),
 .UNSPECIFIED., .F., .F.,
 ( 4, 2, 2, 4 ),
 ( 0.000000000000000000, 0.002450665683189818828, 0.003675998524784728459, 0.004901331366379638524 ),
 .UNSPECIFIED. ) ;
#11586 = DIRECTION ( 'NONE',  ( 0.000000000000000000, -0.8090169943749402348, -0.5877852522924831291 ) ) ;
#11587 = CARTESIAN_POINT ( 'NONE',  ( 3.458734125000001658, 4.235727675282972223E-16, 19.18750000136560629 ) ) ;
#11588 = ADVANCED_FACE ( 'NONE', ( #16054 ), #19971, .T. ) ;
#11589 = CARTESIAN_POINT ( 'NONE',  ( -19.99999999999999645, -9.000000000000003553, 5.000000000000079936 ) ) ;
#11590 = CARTESIAN_POINT ( 'NONE',  ( 4.999999999999999112, 0.000000000000000000, 0.000000000000000000 ) ) ;
#11591 = CARTESIAN_POINT ( 'NONE',  ( 56.09606816583844591, 11.17458954617364242, 11.97181229448534800 ) ) ;
#11592 = EDGE_CURVE ( 'NONE', #23445, #16753, #804, .T. ) ;
#11593 = CARTESIAN_POINT ( 'NONE',  ( -2.445694354108820523, 2.445694354108820523, -3.387499998634403209 ) ) ;
#11594 = CARTESIAN_POINT ( 'NONE',  ( -3.458734124999999437, 0.000000000000000000, 15.68750000136560629 ) ) ;
#11595 = AXIS2_PLACEMENT_3D ( 'NONE', #5229, #7043, #6573 ) ;
#11596 = PLANE ( 'NONE',  #15702 ) ;
#11597 = CARTESIAN_POINT ( 'NONE',  ( -71.15000000109246514, 11.46158073645647235, 13.53841926354352232 ) ) ;
#11598 = CARTESIAN_POINT ( 'NONE',  ( -5.479999999999998650, 7.335634326892644012E-16, 3.059999999999998277 ) ) ;
#11599 = ORIENTED_EDGE ( 'NONE', *, *, #12687, .F. ) ;
#11600 = CARTESIAN_POINT ( 'NONE',  ( -4.175648173966055587, 2.207990556236529844, -3.469390959564062626 ) ) ;
#11601 = CARTESIAN_POINT ( 'NONE',  ( -4.000000000000000000, 0.000000000000000000, 5.425000002731187543 ) ) ;
#11602 = CARTESIAN_POINT ( 'NONE',  ( -71.90000000109247935, 12.06698730000000275, 15.85617417291294196 ) ) ;
#11603 = EDGE_CURVE ( 'NONE', #19299, #19630, #7066, .T. ) ;
#11604 = VERTEX_POINT ( 'NONE', #19738 ) ;
#11605 = EDGE_CURVE ( 'NONE', #18990, #8446, #3339, .T. ) ;
#11606 = ORIENTED_EDGE ( 'NONE', *, *, #9295, .T. ) ;
#11607 = FACE_BOUND ( 'NONE', #11139, .T. ) ;
#11608 = CARTESIAN_POINT ( 'NONE',  ( 52.31250000000000711, 14.00000000000000000, 14.99999999999997691 ) ) ;
#11609 = ORIENTED_EDGE ( 'NONE', *, *, #22075, .T. ) ;
#11610 = CARTESIAN_POINT ( 'NONE',  ( 68.50000000109247367, 10.85617417291294551, 12.93301269999999370 ) ) ;
#11611 = CARTESIAN_POINT ( 'NONE',  ( 1.656854249492384135, -3.999999999999999112, 19.31250000000001776 ) ) ;
#11612 = ORIENTED_EDGE ( 'NONE', *, *, #20402, .F. ) ;
#11613 = CARTESIAN_POINT ( 'NONE',  ( 71.05000000109245661, 9.999999999999998224, 12.93301269999999192 ) ) ;
#11614 = ORIENTED_EDGE ( 'NONE', *, *, #3689, .F. ) ;
#11615 = CARTESIAN_POINT ( 'NONE',  ( -20.00000000000000711, 7.500000000000002665, -19.99999999999999645 ) ) ;
#11616 = CARTESIAN_POINT ( 'NONE',  ( 54.00000000000000711, 12.82842712474617741, 12.17157287525379239 ) ) ;
#11617 = EDGE_CURVE ( 'NONE', #22394, #9212, #10006, .T. ) ;
#11618 = LINE ( 'NONE', #18887, #13463 ) ;
#11619 = DIRECTION ( 'NONE',  ( 0.000000000000000000, 0.000000000000000000, 1.000000000000000000 ) ) ;
#11620 = CARTESIAN_POINT ( 'NONE',  ( 34.99999999999999289, 4.500000000000009770, -50.00000000000000711 ) ) ;
#11621 = CARTESIAN_POINT ( 'NONE',  ( -67.15000000109247935, 11.46158073645647235, 13.53841926354352232 ) ) ;
#11622 = VERTEX_POINT ( 'NONE', #5137 ) ;
#11623 = FACE_OUTER_BOUND ( 'NONE', #2199, .T. ) ;
#11624 = VERTEX_POINT ( 'NONE', #18074 ) ;
#11625 = ADVANCED_FACE ( 'NONE', ( #6951 ), #1183, .F. ) ;
#11626 = DIRECTION ( 'NONE',  ( -1.000000000000000000, 0.000000000000000000, 0.000000000000000000 ) ) ;
#11627 = CARTESIAN_POINT ( 'NONE',  ( 0.2500000000000002220, 4.898587196589412829E-16, -4.000000000000000000 ) ) ;
#11628 = EDGE_CURVE ( 'NONE', #129, #11492, #21827, .T. ) ;
#11629 = EDGE_CURVE ( 'NONE', #8937, #10755, #8855, .T. ) ;
#11630 = ORIENTED_EDGE ( 'NONE', *, *, #21122, .T. ) ;
#11631 = LINE ( 'NONE', #13182, #16639 ) ;
#11632 = CARTESIAN_POINT ( 'NONE',  ( 4.000000000000000888, 4.898587196589412829E-16, 14.62500000273119660 ) ) ;
#11633 = DIRECTION ( 'NONE',  ( 0.000000000000000000, -1.000000000000000000, 0.000000000000000000 ) ) ;
#11634 = AXIS2_PLACEMENT_3D ( 'NONE', #887, #10266, #6655 ) ;
#11635 = CARTESIAN_POINT ( 'NONE',  ( -70.70000000218495018, 11.76776695296636888, 13.23223304703362579 ) ) ;
#11636 = ORIENTED_EDGE ( 'NONE', *, *, #14377, .T. ) ;
#11637 = CARTESIAN_POINT ( 'NONE',  ( -1.656854249492380582, 4.000000000000000000, 1.112500000000000711 ) ) ;
#11638 = ORIENTED_EDGE ( 'NONE', *, *, #15947, .F. ) ;
#11639 = CARTESIAN_POINT ( 'NONE',  ( 71.10000000109246798, 12.06698729999999919, 15.85617417291294196 ) ) ;
#11640 = CARTESIAN_POINT ( 'NONE',  ( -2.828427124746189403, 2.828427124746190291, 14.87500000000000888 ) ) ;
#11641 = CARTESIAN_POINT ( 'NONE',  ( 2.500000000000000000, -1.178949249685214307, 2.042000000000001592 ) ) ;
#11642 = APPLICATION_CONTEXT ( 'automotive_design' ) ;
#11643 = CLOSED_SHELL ( 'NONE', ( #23253, #2640, #17284, #15112, #20038, #10407, #11467, #4371, #4126, #5827, #1761, #13454, #1285, #6904, #16220, #12903, #17894, #7374, #16260, #15703, #12497, #8038, #8325, #1610, #22639, #6146, #19610 ) ) ;
#11644 = VERTEX_POINT ( 'NONE', #23095 ) ;
#11645 = DIRECTION ( 'NONE',  ( 0.000000000000000000, 0.000000000000000000, -1.000000000000000000 ) ) ;
#11646 = CARTESIAN_POINT ( 'NONE',  ( 69.20000000109246230, 7.933012699999995476, 15.85617417291294196 ) ) ;
#11647 = VERTEX_POINT ( 'NONE', #12599 ) ;
#11648 = CYLINDRICAL_SURFACE ( 'NONE', #18688, 8.073750000000021743 ) ;
#11649 = DIRECTION ( 'NONE',  ( 0.000000000000000000, 0.000000000000000000, -1.000000000000000000 ) ) ;
#11650 = CARTESIAN_POINT ( 'NONE',  ( 68.55000000109247082, 8.538419263543524096, 13.53841926354352054 ) ) ;
#11651 = CARTESIAN_POINT ( 'NONE',  ( -2.445694354108819191, 2.445694354108820523, 14.31250000136560452 ) ) ;
#11652 = DIRECTION ( 'NONE',  ( 0.000000000000000000, -5.754033390038005467E-16, -1.000000000000000000 ) ) ;
#11653 = CARTESIAN_POINT ( 'NONE',  ( 6.500000000000001776, 0.6345343291280539644, 5.336307567702092136E-16 ) ) ;
#11654 = ORIENTED_EDGE ( 'NONE', *, *, #7527, .F. ) ;
#11655 = CARTESIAN_POINT ( 'NONE',  ( -1.656854249492381248, -3.999999999999999112, -0.5124999999999969580 ) ) ;
#11656 = PLANE ( 'NONE',  #17337 ) ;
#11657 = CARTESIAN_POINT ( 'NONE',  ( 3.458734125000001214, 4.235727675282971730E-16, 10.93750000136560452 ) ) ;
#11658 = CARTESIAN_POINT ( 'NONE',  ( 0.000000000000000000, 1.464956435139542323, 10.90201369670499076 ) ) ;
#11659 = ADVANCED_FACE ( 'NONE', ( #1654 ), #3216, .T. ) ;
#11660 = PRODUCT ( 'motor', 'motor', '', ( #9737 ) ) ;
#11661 = ORIENTED_EDGE ( 'NONE', *, *, #1004, .T. ) ;
#11662 = CARTESIAN_POINT ( 'NONE',  ( -66.50000000109247367, 9.143825827087049163, 17.06698730000000097 ) ) ;
#11663 = ORIENTED_EDGE ( 'NONE', *, *, #21029, .F. ) ;
#11664 = CARTESIAN_POINT ( 'NONE',  ( 58.50000000000000000, 12.82842712474617741, 12.17157287525379239 ) ) ;
#11665 = CARTESIAN_POINT ( 'NONE',  ( -66.85000000109246798, 7.933012699999995476, 14.99999999999999645 ) ) ;
#11666 = VERTEX_POINT ( 'NONE', #16290 ) ;
#11667 = DIRECTION ( 'NONE',  ( 0.000000000000000000, 1.000000000000000000, -1.224646799147353207E-16 ) ) ;
#11668 = ORIENTED_EDGE ( 'NONE', *, *, #21650, .F. ) ;
#11669 = VERTEX_POINT ( 'NONE', #12241 ) ;
#11670 = CARTESIAN_POINT ( 'NONE',  ( -3.458734124999999437, 0.000000000000000000, 18.68750000136560629 ) ) ;
#11671 = CARTESIAN_POINT ( 'NONE',  ( 56.34375000000000711, 8.757359312880723223, 18.00000000000000355 ) ) ;
#11672 = CARTESIAN_POINT ( 'NONE',  ( -66.10000000109248219, 10.85617417291294551, 12.93301269999999370 ) ) ;
#11673 = CARTESIAN_POINT ( 'NONE',  ( 68.65000000109247935, 12.06698730000000097, 14.99999999999999645 ) ) ;
#11674 = AXIS2_PLACEMENT_3D ( 'NONE', #2719, #19002, #3078 ) ;
#11675 = CARTESIAN_POINT ( 'NONE',  ( -72.14999999999999147, 11.03553390593273598, 12.49999999999999289 ) ) ;
#11676 = CARTESIAN_POINT ( 'NONE',  ( 55.00000000000000711, 15.00000000000000000, 10.00000000000000000 ) ) ;
#11677 = CARTESIAN_POINT ( 'NONE',  ( 59.59143183416158962, 11.31069182806491291, 12.02818770551463778 ) ) ;
#11678 = CARTESIAN_POINT ( 'NONE',  ( -1.506022603841296270, 0.000000000000000000, 0.000000000000000000 ) ) ;
#11679 = CARTESIAN_POINT ( 'NONE',  ( -2.445694354108820523, 2.445694354108820523, 4.862500001365595459 ) ) ;
#11680 = CARTESIAN_POINT ( 'NONE',  ( 26.67945438033275707, -11.25000000000000355, 5.000000000000079936 ) ) ;
#11681 = CARTESIAN_POINT ( 'NONE',  ( 2.828427124746192067, -2.828427124746189847, 11.50000000273119660 ) ) ;
#11682 = FACE_OUTER_BOUND ( 'NONE', #2831, .T. ) ;
#11683 = ORIENTED_EDGE ( 'NONE', *, *, #21636, .F. ) ;
#11684 = CARTESIAN_POINT ( 'NONE',  ( 1.656854249492381470, 4.000000000000000000, 13.68750000000001066 ) ) ;
#11685 = ORIENTED_EDGE ( 'NONE', *, *, #8978, .F. ) ;
#11686 = CARTESIAN_POINT ( 'NONE',  ( 58.27893183416158962, 8.825410453826341595, 11.97181229448535511 ) ) ;
#11687 =( LENGTH_UNIT ( ) NAMED_UNIT ( * ) SI_UNIT ( .MILLI., .METRE. ) );
#11688 = CARTESIAN_POINT ( 'NONE',  ( -1.432654583217640942, -3.458734124999999882, 2.925000001365598123 ) ) ;
#11689 = CARTESIAN_POINT ( 'NONE',  ( -1.432654583217640942, -3.458734124999999882, -0.07499999863440427739 ) ) ;
#11690 = ORIENTED_EDGE ( 'NONE', *, *, #9539, .T. ) ;
#11691 = CARTESIAN_POINT ( 'NONE',  ( 1.656854249492384135, -3.999999999999999112, 13.31250000000001243 ) ) ;
#11692 = AXIS2_PLACEMENT_3D ( 'NONE', #17786, #4846, #12305 ) ;
#11693 = VECTOR ( 'NONE', #17101, 1000.000000000000000 ) ;
#11694 = DIRECTION ( 'NONE',  ( -1.000000000000000000, 0.000000000000000000, -0.000000000000000000 ) ) ;
#11695 = ORIENTED_EDGE ( 'NONE', *, *, #2960, .T. ) ;
#11696 = EDGE_CURVE ( 'NONE', #17148, #22760, #17838, .T. ) ;
#11697 = CARTESIAN_POINT ( 'NONE',  ( -70.30000000218494449, 8.232233047033627571, 16.76776695296636532 ) ) ;
#11698 = CARTESIAN_POINT ( 'NONE',  ( 3.458734125000000770, 4.235727675282972223E-16, -2.512499998634404097 ) ) ;
#11699 =( BOUNDED_CURVE ( )  B_SPLINE_CURVE ( 2, ( #1053, #10437, #8618, #2616, #12109, #23086, #19371, #2965, #14012 ),
 .UNSPECIFIED., .F., .F. ) 
 B_SPLINE_CURVE_WITH_KNOTS ( ( 3, 2, 2, 2, 3 ),
 ( 0.8000000000000000444, 0.8125000000000000000, 0.8249999999999999556, 0.8375000000000000222, 0.8499999999999999778 ),
 .UNSPECIFIED. ) 
 CURVE ( )  GEOMETRIC_REPRESENTATION_ITEM ( )  RATIONAL_B_SPLINE_CURVE ( ( 1.000000000000000000, 0.9238795325112867385, 1.000000000000000000, 0.9238795325112867385, 1.000000000000000000, 0.9238795325112867385, 1.000000000000000000, 0.9238795325112867385, 1.000000000000000000 ) ) 
 REPRESENTATION_ITEM ( '' )  );
#11700 = CARTESIAN_POINT ( 'NONE',  ( 1.872352939448454495E-15, -3.458734125000000770, 17.93750000136560274 ) ) ;
#11701 = EDGE_CURVE ( 'NONE', #11669, #21100, #23374, .T. ) ;
#11702 = CARTESIAN_POINT ( 'NONE',  ( -65.00000000000000000, 9.999999999999998224, 14.99999999999999645 ) ) ;
#11703 = CARTESIAN_POINT ( 'NONE',  ( 68.30000000109247082, 7.933012699999995476, 14.14382582708705094 ) ) ;
#11705 = CARTESIAN_POINT ( 'NONE',  ( 0.2500000000000002220, 5.204748896376250699E-16, -4.250000000000000000 ) ) ;
#11704 = VECTOR ( 'NONE', #14449, 1000.000000000000000 ) ;
#11706 = CARTESIAN_POINT ( 'NONE',  ( 53.09606816583843170, 11.17458954617364242, 11.97181229448534800 ) ) ;
#11707 = AXIS2_PLACEMENT_3D ( 'NONE', #3920, #11258, #14987 ) ;
#11708 = CARTESIAN_POINT ( 'NONE',  ( -3.458734124999999882, -1.432654583217642497, -2.199999998634404541 ) ) ;
#11709 = CARTESIAN_POINT ( 'NONE',  ( 3.458734125000001658, 1.432654583217640498, 11.25000000136560452 ) ) ;
#11710 = CARTESIAN_POINT ( 'NONE',  ( 68.95000000218495018, 8.964466094067285340, 12.49999999999996980 ) ) ;
#11711 = CARTESIAN_POINT ( 'NONE',  ( 55.00000000000000711, 15.00000000000000000, 10.00000000000000000 ) ) ;
#11712 = DIRECTION ( 'NONE',  ( 0.000000000000000000, 0.000000000000000000, -1.000000000000000000 ) ) ;
#11713 = DIRECTION ( 'NONE',  ( -1.224646799147353207E-16, 0.000000000000000000, -1.000000000000000000 ) ) ;
#11714 = ORIENTED_EDGE ( 'NONE', *, *, #12732, .T. ) ;
#11715 = CARTESIAN_POINT ( 'NONE',  ( -1.243802165048909503, 3.900692638707381921, -3.223146290109805800 ) ) ;
#11716 = CARTESIAN_POINT ( 'NONE',  ( 1.656854249492383024, -3.999999999999999112, 4.737500002731186655 ) ) ;
#11717 = CARTESIAN_POINT ( 'NONE',  ( -71.20000000109246230, 10.85617417291294551, 17.06698729999999742 ) ) ;
#11718 = EDGE_LOOP ( 'NONE', ( #2815, #3350, #1861, #20151 ) ) ;
#11719 = ORIENTED_EDGE ( 'NONE', *, *, #17427, .F. ) ;
#11720 = LINE ( 'NONE', #6312, #6029 ) ;
#11721 = CARTESIAN_POINT ( 'NONE',  ( 52.87500000000000711, 7.171572875253794166, 12.17157287525381726 ) ) ;
#11722 = ORIENTED_EDGE ( 'NONE', *, *, #19125, .T. ) ;
#11723 = CARTESIAN_POINT ( 'NONE',  ( 0.5276280594147412240, -4.314175951381924889, -3.320322319201654881 ) ) ;
#11724 = UNCERTAINTY_MEASURE_WITH_UNIT (LENGTH_MEASURE( 1.000000000000000082E-05 ), #11029, 'distance_accuracy_value', 'NONE');
#11725 = EDGE_CURVE ( 'NONE', #8139, #21232, #23430, .T. ) ;
#11726 = AXIS2_PLACEMENT_3D ( 'NONE', #19421, #4945, #3017 ) ;
#11727 = EDGE_CURVE ( 'NONE', #17599, #12610, #8997, .T. ) ;
#11728 = AXIS2_PLACEMENT_3D ( 'NONE', #23313, #21379, #1511 ) ;
#11729 = CARTESIAN_POINT ( 'NONE',  ( 67.45000000109246230, 7.933012699999995476, 14.99999999999999645 ) ) ;
#11730 = CARTESIAN_POINT ( 'NONE',  ( 67.25000000109245946, 12.06698730000000097, 14.99999999999999645 ) ) ;
#11731 = EDGE_CURVE ( 'NONE', #5149, #10094, #8747, .T. ) ;
#11732 = ORIENTED_EDGE ( 'NONE', *, *, #11567, .T. ) ;
#11733 = EDGE_CURVE ( 'NONE', #20008, #21726, #23581, .T. ) ;
#11734 = LINE ( 'NONE', #13167, #11083 ) ;
#11735 = CARTESIAN_POINT ( 'NONE',  ( 57.18750000000000000, 9.999999999999978684, 10.99999999999999645 ) ) ;
#11736 = CARTESIAN_POINT ( 'NONE',  ( 71.65000000218496723, 12.50000000000000000, 16.03553390593273775 ) ) ;
#11737 = CARTESIAN_POINT ( 'NONE',  ( 1.432654583217643163, -3.458734124999999437, 18.75000000136560985 ) ) ;
#11738 = CARTESIAN_POINT ( 'NONE',  ( 47.85166990323382663, -9.000000000000005329, 10.00000000000008882 ) ) ;
#11739 = CARTESIAN_POINT ( 'NONE',  ( 1.519999999999999574, 8.279592079675421725E-16, 6.760799999999997034 ) ) ;
#11740 = VERTEX_POINT ( 'NONE', #18658 ) ;
#11741 = DIRECTION ( 'NONE',  ( -1.000000000000000000, 0.000000000000000000, -0.000000000000000000 ) ) ;
#11742 = CARTESIAN_POINT ( 'NONE',  ( 0.000000000000000000, 0.000000000000000000, 0.000000000000000000 ) ) ;
#11743 = CARTESIAN_POINT ( 'NONE',  ( 1.506022603841296714, 8.263794135966437014E-16, 6.735000000000022524 ) ) ;
#11744 = VERTEX_POINT ( 'NONE', #10909 ) ;
#11745 = CARTESIAN_POINT ( 'NONE',  ( 69.35000000218497007, 11.03553390593273420, 17.50000000000000711 ) ) ;
#11746 = LINE ( 'NONE', #23077, #23656 ) ;
#11747 = DIRECTION ( 'NONE',  ( -1.000000000000000000, -0.000000000000000000, -0.000000000000000000 ) ) ;
#11748 = ADVANCED_FACE ( 'NONE', ( #3921 ), #12939, .F. ) ;
#11749 = CARTESIAN_POINT ( 'NONE',  ( 47.84242505928347100, -8.974600000000002353, 5.000000000000079936 ) ) ;
#11750 = EDGE_LOOP ( 'NONE', ( #10950, #12979, #23194, #9430 ) ) ;
#11751 = CARTESIAN_POINT ( 'NONE',  ( 50.00000000000000000, 15.00000000000003375, 10.00000000000008882 ) ) ;
#11752 = ORIENTED_EDGE ( 'NONE', *, *, #21604, .T. ) ;
#11753 = CARTESIAN_POINT ( 'NONE',  ( 70.80000000109245661, 9.143825827087052716, 12.93301269999999192 ) ) ;
#11754 = EDGE_CURVE ( 'NONE', #7010, #13210, #2245, .T. ) ;
#11755 = LINE ( 'NONE', #2611, #10643 ) ;
#11756 = CARTESIAN_POINT ( 'NONE',  ( 54.99999999999992895, 15.00000000000000000, 1.836970198721037478E-15 ) ) ;
#11757 = LINE ( 'NONE', #22374, #7271 ) ;
#11758 = CARTESIAN_POINT ( 'NONE',  ( -4.000000000000000000, -2.309401076758512694, -3.433295621305382461 ) ) ;
#11759 = CARTESIAN_POINT ( 'NONE',  ( 69.85000000109246798, 9.999999999999998224, 17.06698730000000097 ) ) ;
#11760 = EDGE_CURVE ( 'NONE', #14122, #10129, #7718, .T. ) ;
#11761 = VERTEX_POINT ( 'NONE', #14623 ) ;
#11762 = ADVANCED_FACE ( 'NONE', ( #3812 ), #9106, .F. ) ;
#11763 = CARTESIAN_POINT ( 'NONE',  ( 19.99999999999998934, 4.500000000000001776, -50.00000000000000000 ) ) ;
#11764 = CYLINDRICAL_SURFACE ( 'NONE', #11069, 2.499999999999998668 ) ;
#11765 = CARTESIAN_POINT ( 'NONE',  ( 71.20000000109246230, 12.06698730000000275, 14.14382582708705094 ) ) ;
#11766 = CARTESIAN_POINT ( 'NONE',  ( 1.025207404391860050E-15, 3.458734125000000326, 14.18750000136560452 ) ) ;
#11767 = DIRECTION ( 'NONE',  ( 0.000000000000000000, 1.000000000000000000, 3.491481338843133355E-15 ) ) ;
#11768 = CARTESIAN_POINT ( 'NONE',  ( -20.00005080000000035, 0.000000000000000000, 0.000000000000000000 ) ) ;
#11769 = ORIENTED_EDGE ( 'NONE', *, *, #12888, .F. ) ;
#11770 = CARTESIAN_POINT ( 'NONE',  ( 4.000000000000000000, 4.898587196589412829E-16, 2.800000000000002043 ) ) ;
#11771 = CARTESIAN_POINT ( 'NONE',  ( -1.696909521094715823, -2.338219870597463945, 10.00000000000008882 ) ) ;
#11772 = FACE_OUTER_BOUND ( 'NONE', #10453, .T. ) ;
#11773 = CARTESIAN_POINT ( 'NONE',  ( 71.40000000218495302, 9.999999999999998224, 12.49999999999999289 ) ) ;
#11774 = ORIENTED_EDGE ( 'NONE', *, *, #18099, .F. ) ;
#11775 = CARTESIAN_POINT ( 'NONE',  ( 65.00000000000000000, 9.999999999999998224, 12.49999999999999289 ) ) ;
#11776 = ORIENTED_EDGE ( 'NONE', *, *, #12082, .T. ) ;
#11777 = AXIS2_PLACEMENT_3D ( 'NONE', #10466, #16189, #10930 ) ;
#11778 = CARTESIAN_POINT ( 'NONE',  ( -68.70000000109246230, 10.85617417291294551, 12.93301269999999370 ) ) ;
#11779 = EDGE_LOOP ( 'NONE', ( #1305, #20865, #22401, #3161, #13814 ) ) ;
#11780 = DIRECTION ( 'NONE',  ( 0.000000000000000000, 0.000000000000000000, 1.000000000000000000 ) ) ;
#11781 = ORIENTED_EDGE ( 'NONE', *, *, #15566, .F. ) ;
#11782 = CIRCLE ( 'NONE', #11796, 4.000000000000000888 ) ;
#11783 = EDGE_LOOP ( 'NONE', ( #13685, #22598, #681, #9850 ) ) ;
#11784 = CARTESIAN_POINT ( 'NONE',  ( 2.445694354108821411, 2.445694354108820523, 17.31250000136560629 ) ) ;
#11785 = CARTESIAN_POINT ( 'NONE',  ( 52.21875000000002842, 13.00000000000000711, 16.24264068711927322 ) ) ;
#11786 = VECTOR ( 'NONE', #5704, 1000.000000000000000 ) ;
#11787 = CIRCLE ( 'NONE', #1024, 8.749000000000002331 ) ;
#11788 = CARTESIAN_POINT ( 'NONE',  ( -66.20000000109247651, 12.06698730000000275, 14.14382582708705094 ) ) ;
#11789 = CARTESIAN_POINT ( 'NONE',  ( 67.75000000109247367, 11.46158073645647235, 13.53841926354352232 ) ) ;
#11790 = EDGE_CURVE ( 'NONE', #669, #4306, #1957, .T. ) ;
#11791 = EDGE_CURVE ( 'NONE', #5947, #6574, #20296, .T. ) ;
#11792 = CARTESIAN_POINT ( 'NONE',  ( -67.25000000109245946, 12.06698730000000097, 14.99999999999999645 ) ) ;
#11793 = DIRECTION ( 'NONE',  ( 0.000000000000000000, 0.000000000000000000, -1.000000000000000000 ) ) ;
#11794 = CARTESIAN_POINT ( 'NONE',  ( 56.21643183416158251, 12.97181229448535689, 16.31069182806490758 ) ) ;
#11795 = DIRECTION ( 'NONE',  ( 7.010384997569515515E-32, 1.000000000000000000, -3.469446951953615175E-16 ) ) ;
#11796 = AXIS2_PLACEMENT_3D ( 'NONE', #21217, #14313, #3029 ) ;
#11797 = CARTESIAN_POINT ( 'NONE',  ( -2.445694354108819635, -2.445694354108820967, 2.112500001365596791 ) ) ;
#11798 = CARTESIAN_POINT ( 'NONE',  ( -19.99999999999999645, -9.000000000000003553, 5.000000000000079936 ) ) ;
#11799 = CARTESIAN_POINT ( 'NONE',  ( -1.656854249492380138, -3.999999999999999112, 12.31250000273119660 ) ) ;
#11800 = DIRECTION ( 'NONE',  ( 0.000000000000000000, 0.5877852522924743583, -0.8090169943749467851 ) ) ;
#11801 = AXIS2_PLACEMENT_3D ( 'NONE', #18056, #10426, #3442 ) ;
#11802 = AXIS2_PLACEMENT_3D ( 'NONE', #11962, #435, #15079 ) ;
#11803 = ORIENTED_EDGE ( 'NONE', *, *, #3401, .F. ) ;
#11804 = CARTESIAN_POINT ( 'NONE',  ( -12.00000000000000000, 1.469576158976823947E-15, -3.999999999999998224 ) ) ;
#11805 = ORIENTED_EDGE ( 'NONE', *, *, #5067, .F. ) ;
#11806 = CARTESIAN_POINT ( 'NONE',  ( 59.96643183416158251, 7.028187705514638672, 13.68930817193508531 ) ) ;
#11807 = CARTESIAN_POINT ( 'NONE',  ( -3.458734124999999882, -1.432654583217642497, 2.800000001365598123 ) ) ;
#11808 = CARTESIAN_POINT ( 'NONE',  ( -1.432654583217640942, -3.458734124999999882, -1.074999998634403431 ) ) ;
#11809 = ORIENTED_EDGE ( 'NONE', *, *, #18424, .T. ) ;
#11810 = DIRECTION ( 'NONE',  ( 0.000000000000000000, 0.000000000000000000, -1.000000000000000000 ) ) ;
#11811 = DIRECTION ( 'NONE',  ( -1.000000000000000000, 0.000000000000000000, 0.000000000000000000 ) ) ;
#11812 = CARTESIAN_POINT ( 'NONE',  ( 4.000000000000000888, 1.656854249492381248, 14.56250000000000888 ) ) ;
#11813 = ORIENTED_EDGE ( 'NONE', *, *, #14552, .F. ) ;
#11814 = AXIS2_PLACEMENT_3D ( 'NONE', #6942, #1527, #23570 ) ;
#11815 = CARTESIAN_POINT ( 'NONE',  ( -69.55000000218495870, 7.499999999999995559, 16.03553390593273420 ) ) ;
#11816 = DIRECTION ( 'NONE',  ( -1.000000000000000000, -0.000000000000000000, -0.000000000000000000 ) ) ;
#11817 = CARTESIAN_POINT ( 'NONE',  ( -3.802871176606132497, -5.309964801958124703, -3.686277791023380601 ) ) ;
#11818 = COLOUR_RGB ( '', 0.40784314, 0.44705882, 0.49803922) ;
#11819 = CARTESIAN_POINT ( 'NONE',  ( -1.432654583217639166, 3.458734125000000770, 19.50000000136560629 ) ) ;
#11820 = LINE ( 'NONE', #15417, #15083 ) ;
#11821 = CARTESIAN_POINT ( 'NONE',  ( 70.95000000109247651, 11.46158073645647235, 13.53841926354352232 ) ) ;
#11822 = CARTESIAN_POINT ( 'NONE',  ( 70.95000000218495018, 11.03553390593269867, 17.50000000000003908 ) ) ;
#11823 = CARTESIAN_POINT ( 'NONE',  ( 55.34606816583843880, 8.825410453826357582, 18.02818770551464667 ) ) ;
#11824 = PRODUCT_RELATED_PRODUCT_CATEGORY ( 'part', '', ( #11248 ) ) ;
#11825 = CARTESIAN_POINT ( 'NONE',  ( 2.445694354108820967, -2.445694354108820079, 5.362500001365596347 ) ) ;
#11826 = FACE_OUTER_BOUND ( 'NONE', #19199, .T. ) ;
#11827 = CARTESIAN_POINT ( 'NONE',  ( 67.64999999999999147, 11.03553390593272887, 17.50000000000001066 ) ) ;
#11828 = CARTESIAN_POINT ( 'NONE',  ( -68.60000000109246798, 9.143825827087052716, 12.93301269999999192 ) ) ;
#11829 = AXIS2_PLACEMENT_3D ( 'NONE', #18180, #14614, #16044 ) ;
#11830 = EDGE_CURVE ( 'NONE', #17305, #10717, #13081, .T. ) ;
#11831 = LINE ( 'NONE', #10270, #6637 ) ;
#11832 = CARTESIAN_POINT ( 'NONE',  ( 35.00000000000000000, 7.500000000000001776, -20.00000000000000355 ) ) ;
#11833 = ORIENTED_EDGE ( 'NONE', *, *, #11868, .T. ) ;
#11834 = LINE ( 'NONE', #18867, #3066 ) ;
#11835 = CARTESIAN_POINT ( 'NONE',  ( -4.000000000000000000, 0.000000000000000000, 3.425000002731189319 ) ) ;
#11836 = EDGE_LOOP ( 'NONE', ( #19312, #12581, #446, #16519 ) ) ;
#11837 = VERTEX_POINT ( 'NONE', #4049 ) ;
#11838 = CYLINDRICAL_SURFACE ( 'NONE', #9477, 4.000000000000001776 ) ;
#11839 = VECTOR ( 'NONE', #8984, 1000.000000000000000 ) ;
#11840 = LINE ( 'NONE', #662, #9880 ) ;
#11841 = ORIENTED_EDGE ( 'NONE', *, *, #19459, .T. ) ;
#11842 = CARTESIAN_POINT ( 'NONE',  ( -0.7060087303327398089, -11.25000000000000355, 10.00000000000008882 ) ) ;
#11843 = CARTESIAN_POINT ( 'NONE',  ( 67.95000000109247651, 11.46158073645647235, 16.46158073645647235 ) ) ;
#11844 = VECTOR ( 'NONE', #21218, 1000.000000000000000 ) ;
#11845 = CARTESIAN_POINT ( 'NONE',  ( 68.40000000109246514, 7.933012699999995476, 15.85617417291294196 ) ) ;
#11846 = PRODUCT ( 'BR-005', 'BR-005', '', ( #21590 ) ) ;
#11847 = VERTEX_POINT ( 'NONE', #5969 ) ;
#11848 = PRODUCT_DEFINITION_FORMATION_WITH_SPECIFIED_SOURCE ( 'ANY', '', #127, .NOT_KNOWN. ) ;
#11849 = DIRECTION ( 'NONE',  ( 1.000000000000000000, 7.703719777548943412E-32, 0.000000000000000000 ) ) ;
#11850 = VECTOR ( 'NONE', #10869, 1000.000000000000000 ) ;
#11851 = CARTESIAN_POINT ( 'NONE',  ( 56.90625000000000711, 13.99999999999999289, 13.34314575050759544 ) ) ;
#11852 = CARTESIAN_POINT ( 'NONE',  ( 4.000000000000000888, 4.898587196589412829E-16, 12.62500000273119660 ) ) ;
#11853 = CARTESIAN_POINT ( 'NONE',  ( 3.458734125000001214, 4.235727675282971730E-16, 17.93750000136560274 ) ) ;
#11854 = CYLINDRICAL_SURFACE ( 'NONE', #4785, 2.500000000000002220 ) ;
#11855 = EDGE_CURVE ( 'NONE', #10715, #7612, #6889, .T. ) ;
#11856 = DIRECTION ( 'NONE',  ( 1.000000000000000000, 0.000000000000000000, 0.000000000000000000 ) ) ;
#11857 = EDGE_LOOP ( 'NONE', ( #15782, #13038, #20817, #4416 ) ) ;
#11858 = DIRECTION ( 'NONE',  ( 0.000000000000000000, 0.000000000000000000, -1.000000000000000000 ) ) ;
#11859 = EDGE_CURVE ( 'NONE', #8586, #19009, #9233, .T. ) ;
#11860 = CARTESIAN_POINT ( 'NONE',  ( -2.828427124746188515, -2.828427124746190735, 12.12500000000001066 ) ) ;
#11861 = DIRECTION ( 'NONE',  ( 1.000000000000000000, 0.000000000000000000, 0.000000000000000000 ) ) ;
#11862 = AXIS2_PLACEMENT_3D ( 'NONE', #23597, #3358, #14641 ) ;
#11863 = ORIENTED_EDGE ( 'NONE', *, *, #19440, .F. ) ;
#11864 = VECTOR ( 'NONE', #7884, 1000.000000000000114 ) ;
#11865 = CARTESIAN_POINT ( 'NONE',  ( 4.024499207728657879, 2.323545700935571556, -3.572172305156506411 ) ) ;
#11866 = CARTESIAN_POINT ( 'NONE',  ( 9.546947090716562556, -8.974600000000002353, 10.00000000000008882 ) ) ;
#11867 = CARTESIAN_POINT ( 'NONE',  ( -2.828427124746188515, -2.828427124746190735, 11.25000000273119660 ) ) ;
#11868 = EDGE_CURVE ( 'NONE', #21099, #22731, #21997, .T. ) ;
#11869 = DIRECTION ( 'NONE',  ( -1.224646799147353207E-16, 0.000000000000000000, -1.000000000000000000 ) ) ;
#11870 = ORIENTED_EDGE ( 'NONE', *, *, #17587, .F. ) ;
#11871 = CARTESIAN_POINT ( 'NONE',  ( 3.250000000000003109, 5.629165124598848102, 1.734723475976807094E-15 ) ) ;
#11872 = ORIENTED_EDGE ( 'NONE', *, *, #15305, .F. ) ;
#11873 = AXIS2_PLACEMENT_3D ( 'NONE', #16441, #20005, #20118 ) ;
#11874 = FACE_OUTER_BOUND ( 'NONE', #1979, .T. ) ;
#11875 = AXIS2_PLACEMENT_3D ( 'NONE', #18753, #7985, #425 ) ;
#11876 = CARTESIAN_POINT ( 'NONE',  ( 1.656854249492384135, -3.999999999999999112, 12.31250000000001243 ) ) ;
#11877 = CARTESIAN_POINT ( 'NONE',  ( 69.60000000218495586, 7.499999999999996447, 14.99999999999999645 ) ) ;
#11878 = CARTESIAN_POINT ( 'NONE',  ( 6.499999999999999112, 2.531211054341943711, -3.440493080744402299 ) ) ;
#11879 = CARTESIAN_POINT ( 'NONE',  ( -4.000000000000000000, 4.898587196589412829E-16, 19.04999999999996874 ) ) ;
#11880 = CARTESIAN_POINT ( 'NONE',  ( 66.40000000109247935, 12.06698729999999919, 14.14382582708705094 ) ) ;
#11881 = VERTEX_POINT ( 'NONE', #16518 ) ;
#11882 = CIRCLE ( 'NONE', #16837, 6.499999999999999112 ) ;
#11883 = DIRECTION ( 'NONE',  ( -1.000000000000000000, 0.000000000000000000, 0.000000000000000000 ) ) ;
#11884 = DIRECTION ( 'NONE',  ( -1.000000000000000000, -0.000000000000000000, 0.000000000000000000 ) ) ;
#11885 = CARTESIAN_POINT ( 'NONE',  ( 69.20000000109246230, 7.933012699999995476, 15.85617417291294196 ) ) ;
#11886 = CARTESIAN_POINT ( 'NONE',  ( -3.458734124999998993, -1.432654583217642497, 11.50000000136560629 ) ) ;
#11887 = AXIS2_PLACEMENT_3D ( 'NONE', #18630, #2215, #2341 ) ;
#11888 = DIRECTION ( 'NONE',  ( 1.000000000000000000, 0.000000000000000000, 0.000000000000000000 ) ) ;
#11889 = DIRECTION ( 'NONE',  ( 0.000000000000000000, 0.000000000000000000, 1.000000000000000000 ) ) ;
#11890 = VECTOR ( 'NONE', #397, 999.9999999999998863 ) ;
#11891 = ORIENTED_EDGE ( 'NONE', *, *, #22805, .F. ) ;
#11892 = CARTESIAN_POINT ( 'NONE',  ( 7.347880794884118750E-16, -4.000000000000000000, 2.550000000000002043 ) ) ;
#11893 = EDGE_CURVE ( 'NONE', #16036, #21124, #94, .T. ) ;
#11894 = DIRECTION ( 'NONE',  ( -0.3420201433256622181, 0.9396926207859106484, 1.232595164407828100E-31 ) ) ;
#11895 = CARTESIAN_POINT ( 'NONE',  ( -1.432654583217638944, 3.458734125000000326, 11.25000000136560452 ) ) ;
#11896 = CARTESIAN_POINT ( 'NONE',  ( 118.3095189484530181, -2.399706452296352932, 60.00000000000021316 ) ) ;
#11897 = ORIENTED_EDGE ( 'NONE', *, *, #1743, .T. ) ;
#11898 = CARTESIAN_POINT ( 'NONE',  ( -66.25000000109247367, 12.06698730000000097, 14.99999999999999645 ) ) ;
#11899 = ORIENTED_EDGE ( 'NONE', *, *, #23541, .F. ) ;
#11900 = CARTESIAN_POINT ( 'NONE',  ( -66.95000000109246230, 8.538419263543524096, 13.53841926354352054 ) ) ;
#11901 = ADVANCED_FACE ( 'NONE', ( #4643, #15451 ), #2596, .T. ) ;
#11902 = VERTEX_POINT ( 'NONE', #17236 ) ;
#11903 = DIRECTION ( 'NONE',  ( 0.000000000000000000, 0.000000000000000000, -1.000000000000000000 ) ) ;
#11904 = ORIENTED_EDGE ( 'NONE', *, *, #10742, .F. ) ;
#11905 = ADVANCED_FACE ( 'NONE', ( #9939 ), #7672, .T. ) ;
#11906 = VERTEX_POINT ( 'NONE', #16994 ) ;
#11907 = CARTESIAN_POINT ( 'NONE',  ( -2.445694354108819191, 2.445694354108820523, 13.56250000136560629 ) ) ;
#11908 = CARTESIAN_POINT ( 'NONE',  ( -4.000000000000000000, 0.000000000000000000, -0.5749999972688123462 ) ) ;
#11909 = CIRCLE ( 'NONE', #9991, 5.384454397937118664 ) ;
#11910 = VECTOR ( 'NONE', #23485, 1000.000000000000000 ) ;
#11911 = FACE_OUTER_BOUND ( 'NONE', #958, .T. ) ;
#11912 = VECTOR ( 'NONE', #13917, 1000.000000000000114 ) ;
#11913 = CARTESIAN_POINT ( 'NONE',  ( 35.00000000000000000, 4.500000000000001776, -20.00000000000000355 ) ) ;
#11914 = CARTESIAN_POINT ( 'NONE',  ( -67.85000000109246798, 9.999999999999998224, 12.93301269999999192 ) ) ;
#11915 =( BOUNDED_CURVE ( )  B_SPLINE_CURVE ( 2, ( #8741, #6700, #4547, #8622, #14015, #13666, #10201, #4662, #21274 ),
 .UNSPECIFIED., .F., .F. ) 
 B_SPLINE_CURVE_WITH_KNOTS ( ( 3, 2, 2, 2, 3 ),
 ( 0.4374999999999995004, 0.4531249999999993894, 0.4687499999999993339, 0.4843749999999992228, 0.4999999999999991118 ),
 .UNSPECIFIED. ) 
 CURVE ( )  GEOMETRIC_REPRESENTATION_ITEM ( )  RATIONAL_B_SPLINE_CURVE ( ( 1.000000000000002442, 0.9238795325112842960, 1.000000000000000000, 0.9238795325112867385, 1.000000000000000000, 0.9238795325112867385, 1.000000000000000000, 0.9238795325112910684, 0.9999999999999956701 ) ) 
 REPRESENTATION_ITEM ( '' )  );
#11916 = CARTESIAN_POINT ( 'NONE',  ( 60.00000000000000711, 15.00000000000000000, 19.99999999999999645 ) ) ;
#11917 = CARTESIAN_POINT ( 'NONE',  ( 58.65393183416157541, 5.971812294485358663, 16.58880310854675599 ) ) ;
#11918 = DIRECTION ( 'NONE',  ( 1.000000000000000000, 0.000000000000000000, 0.000000000000000000 ) ) ;
#11919 = CARTESIAN_POINT ( 'NONE',  ( -1.432654583217641164, -3.458734125000000326, 5.175000001365595459 ) ) ;
#11920 = LINE ( 'NONE', #11798, #3986 ) ;
#11921 = CARTESIAN_POINT ( 'NONE',  ( -3.999999999999999112, 1.656854249492380804, 10.06250000273119660 ) ) ;
#11922 = CARTESIAN_POINT ( 'NONE',  ( 28.99286915928345110, -8.974600000000002353, 5.000000000000079936 ) ) ;
#11923 = AXIS2_PLACEMENT_3D ( 'NONE', #8051, #8402, #19159 ) ;
#11924 = EDGE_LOOP ( 'NONE', ( #14014, #7674, #17036, #15140 ) ) ;
#11925 = CARTESIAN_POINT ( 'NONE',  ( 1.656854249492381470, 4.000000000000000000, 16.81250000273119838 ) ) ;
#11926 = ORIENTED_EDGE ( 'NONE', *, *, #20158, .T. ) ;
#11927 = CARTESIAN_POINT ( 'NONE',  ( 52.27893183416158251, 8.825410453826341595, 11.97181229448535511 ) ) ;
#11928 = DIRECTION ( 'NONE',  ( 0.000000000000000000, 0.000000000000000000, 1.000000000000000000 ) ) ;
#11929 = EDGE_CURVE ( 'NONE', #15611, #7937, #2832, .T. ) ;
#11930 = CARTESIAN_POINT ( 'NONE',  ( 1.432654583217639832, 3.458734125000000326, 2.425000001365597679 ) ) ;
#11931 = ADVANCED_FACE ( 'NONE', ( #2365, #10180 ), #18894, .F. ) ;
#11932 = CARTESIAN_POINT ( 'NONE',  ( -2.445694354108820523, 2.445694354108820523, -0.3874999986344038194 ) ) ;
#11933 = EDGE_LOOP ( 'NONE', ( #22729, #11481, #195, #12254 ) ) ;
#11934 = DIRECTION ( 'NONE',  ( 1.000000000000000000, 0.000000000000000000, 0.000000000000000000 ) ) ;
#11935 = ADVANCED_FACE ( 'NONE', ( #11623 ), #13646, .T. ) ;
#11936 = FILL_AREA_STYLE_COLOUR ( '', #16010 ) ;
#11937 = ORIENTED_EDGE ( 'NONE', *, *, #9794, .T. ) ;
#11938 = CARTESIAN_POINT ( 'NONE',  ( 72.50000000000000000, 9.999999999999998224, 12.49999999999999289 ) ) ;
#11939 = ORIENTED_EDGE ( 'NONE', *, *, #14986, .F. ) ;
#11940 = CARTESIAN_POINT ( 'NONE',  ( 50.84606816583843880, 8.411196891453267099, 19.02818770551464667 ) ) ;
#11941 = CARTESIAN_POINT ( 'NONE',  ( -69.65000000218496723, 7.499999999999995559, 13.96446609406725692 ) ) ;
#11942 = CARTESIAN_POINT ( 'NONE',  ( 6.353591512924457348E-16, -3.458734125000000770, -2.762499998634404097 ) ) ;
#11943 = CARTESIAN_POINT ( 'NONE',  ( 4.000000000000000888, 4.898587196589412829E-16, 15.50000000000001066 ) ) ;
#11944 = CARTESIAN_POINT ( 'NONE',  ( 66.69999999999998863, 12.50000000000000000, 14.99999999999999645 ) ) ;
#11945 = CARTESIAN_POINT ( 'NONE',  ( 4.000000000000001776, -1.656854249492379694, 12.56250000273119660 ) ) ;
#11946 = CYLINDRICAL_SURFACE ( 'NONE', #23076, 8.749000000000002331 ) ;
#11947 = CARTESIAN_POINT ( 'NONE',  ( 69.30000000109247082, 10.85617417291294551, 12.93301269999999370 ) ) ;
#11948 = CARTESIAN_POINT ( 'NONE',  ( -2.413812496766191806, -9.000000000000001776, 10.00000000000008882 ) ) ;
#11949 = CARTESIAN_POINT ( 'NONE',  ( 52.34606816583843880, 8.825410453826357582, 18.02818770551464667 ) ) ;
#11950 = CARTESIAN_POINT ( 'NONE',  ( 3.458734125000000770, 4.235727675282972223E-16, 0.4875000013655969577 ) ) ;
#11951 = CARTESIAN_POINT ( 'NONE',  ( -2.445694354108818303, -2.445694354108820967, 12.81250000136560629 ) ) ;
#11952 = CARTESIAN_POINT ( 'NONE',  ( -70.10000000109246798, 7.933012699999995476, 14.14382582708705094 ) ) ;
#11953 = CARTESIAN_POINT ( 'NONE',  ( 4.101954839143059139, -2.368264730582948285, -3.681130640444269631 ) ) ;
#11954 = FACE_OUTER_BOUND ( 'NONE', #4709, .T. ) ;
#11955 = VERTEX_POINT ( 'NONE', #20908 ) ;
#11956 = CARTESIAN_POINT ( 'NONE',  ( 5.000000000000000000, 5.400000000000000355, 0.000000000000000000 ) ) ;
#11957 = FILL_AREA_STYLE_COLOUR ( '', #13390 ) ;
#11958 = CARTESIAN_POINT ( 'NONE',  ( -1.656854249492380804, 4.000000000000000000, 3.237500002731188875 ) ) ;
#11959 = ORIENTED_EDGE ( 'NONE', *, *, #5761, .F. ) ;
#11960 = ORIENTED_EDGE ( 'NONE', *, *, #21194, .T. ) ;
#11961 = DIRECTION ( 'NONE',  ( 0.000000000000000000, 0.000000000000000000, 1.000000000000000000 ) ) ;
#11962 = CARTESIAN_POINT ( 'NONE',  ( 25.85127650928345489, -8.974600000000002353, 5.000000000000079936 ) ) ;
#11963 = ORIENTED_EDGE ( 'NONE', *, *, #10889, .F. ) ;
#11964 = CARTESIAN_POINT ( 'NONE',  ( 3.472371940585993855, 2.614027278893175321, -3.320322319201766792 ) ) ;
#11965 = UNCERTAINTY_MEASURE_WITH_UNIT (LENGTH_MEASURE( 1.000000000000000082E-05 ), #10127, 'distance_accuracy_value', 'NONE');
#11966 = CARTESIAN_POINT ( 'NONE',  ( 68.60000000109248219, 12.06698730000000275, 14.14382582708705094 ) ) ;
#11967 = EDGE_CURVE ( 'NONE', #16436, #6393, #12661, .T. ) ;
#11968 = CARTESIAN_POINT ( 'NONE',  ( 66.95000000109246230, 8.538419263543524096, 13.53841926354352054 ) ) ;
#11969 = ORIENTED_EDGE ( 'NONE', *, *, #8960, .F. ) ;
#11970 = DIRECTION ( 'NONE',  ( -1.000000000000000000, 0.000000000000000000, -0.000000000000000000 ) ) ;
#11971 = CARTESIAN_POINT ( 'NONE',  ( 56.53125000000000711, 11.65685424949239923, 18.99999999999998934 ) ) ;
#11972 = CARTESIAN_POINT ( 'NONE',  ( 71.45000000218495018, 11.03553390593275374, 12.50000000000001243 ) ) ;
#11973 = CARTESIAN_POINT ( 'NONE',  ( 72.50000000000000000, 9.999999999999998224, 14.99999999999999645 ) ) ;
#11974 = CARTESIAN_POINT ( 'NONE',  ( -9.311853653233800543, -9.000000000000005329, 10.00000000000008882 ) ) ;
#11975 = DIRECTION ( 'NONE',  ( 1.000000000000000000, 0.000000000000000000, 0.000000000000000000 ) ) ;
#11976 = ORIENTED_EDGE ( 'NONE', *, *, #15985, .F. ) ;
#11977 = DIRECTION ( 'NONE',  ( 1.000000000000000000, 0.000000000000000000, 0.000000000000000000 ) ) ;
#11978 = FACE_OUTER_BOUND ( 'NONE', #20059, .T. ) ;
#11979 = CARTESIAN_POINT ( 'NONE',  ( 2.000000000000001776, 0.000000000000000000, 0.000000000000000000 ) ) ;
#11980 = EDGE_LOOP ( 'NONE', ( #13277, #10857, #16913, #8559 ) ) ;
#11981 = CARTESIAN_POINT ( 'NONE',  ( 1.747541505913279281, -3.837784562140273081, -3.503702292528912299 ) ) ;
#11982 = CARTESIAN_POINT ( 'NONE',  ( 4.999999999999999112, 8.461683424509345741, -2.223716399045483350 ) ) ;
#11983 = AXIS2_PLACEMENT_3D ( 'NONE', #10424, #19359, #6799 ) ;
#11984 = CARTESIAN_POINT ( 'NONE',  ( 71.40000000218495302, 9.999999999999998224, 12.49999999999999289 ) ) ;
#11985 = ORIENTED_EDGE ( 'NONE', *, *, #10383, .T. ) ;
#11986 = CARTESIAN_POINT ( 'NONE',  ( 2.696295709017752618, 5.948846446048902337, 4.712891318522927087E-15 ) ) ;
#11987 = VERTEX_POINT ( 'NONE', #17471 ) ;
#11988 = DIRECTION ( 'NONE',  ( 0.3420201433256622736, 0.9396926207859106484, 0.000000000000000000 ) ) ;
#11989 = CARTESIAN_POINT ( 'NONE',  ( 71.35000000218494165, 8.964466094067258695, 12.49999999999999289 ) ) ;
#11990 = EDGE_CURVE ( 'NONE', #5746, #9385, #20797, .T. ) ;
#11991 = CARTESIAN_POINT ( 'NONE',  ( -1.656854249492380138, -3.999999999999999112, 16.18750000000001066 ) ) ;
#11992 = EDGE_CURVE ( 'NONE', #17728, #4019, #6449, .T. ) ;
#11993 = DIRECTION ( 'NONE',  ( 1.000000000000000000, 0.000000000000000000, 0.000000000000000000 ) ) ;
#11994 = CARTESIAN_POINT ( 'NONE',  ( 66.10000000109246798, 7.933012699999995476, 14.14382582708705094 ) ) ;
#11995 = ORIENTED_EDGE ( 'NONE', *, *, #8808, .T. ) ;
#11996 = LINE ( 'NONE', #10442, #11472 ) ;
#11997 = DIRECTION ( 'NONE',  ( 1.000000000000000000, -0.000000000000000000, -0.000000000000000000 ) ) ;
#11998 = EDGE_CURVE ( 'NONE', #313, #20062, #22961, .T. ) ;
#11999 = CARTESIAN_POINT ( 'NONE',  ( 71.25000000109247367, 12.06698730000000097, 14.99999999999999645 ) ) ;
#12000 = CARTESIAN_POINT ( 'NONE',  ( -3.458734124999998993, 0.000000000000000000, 12.43750000136560629 ) ) ;
#12001 = LINE ( 'NONE', #14019, #7846 ) ;
#12002 = DIRECTION ( 'NONE',  ( 1.224646799147353207E-16, -0.000000000000000000, 1.000000000000000000 ) ) ;
#12003 = VERTEX_POINT ( 'NONE', #566 ) ;
#12004 = CARTESIAN_POINT ( 'NONE',  ( 4.000000000000000000, 1.656854249492381248, -2.137499999999997957 ) ) ;
#12005 = CIRCLE ( 'NONE', #504, 4.000000000000001776 ) ;
#12006 = CARTESIAN_POINT ( 'NONE',  ( 2.500000000000000000, 2.357898499370431722, -2.818925648462311528E-15 ) ) ;
#12007 = LINE ( 'NONE', #19272, #3560 ) ;
#12008 = DIRECTION ( 'NONE',  ( -1.000000000000000000, -0.000000000000000000, -0.000000000000000000 ) ) ;
#12009 = ORIENTED_EDGE ( 'NONE', *, *, #1436, .T. ) ;
#12010 = DIRECTION ( 'NONE',  ( 1.000000000000000000, 0.000000000000000000, 0.000000000000000000 ) ) ;
#12011 = ORIENTED_EDGE ( 'NONE', *, *, #22673, .T. ) ;
#12012 = CARTESIAN_POINT ( 'NONE',  ( -66.35000000109246798, 11.46158073645647235, 13.53841926354352232 ) ) ;
#12013 = ORIENTED_EDGE ( 'NONE', *, *, #10533, .F. ) ;
#12014 = DIRECTION ( 'NONE',  ( 0.000000000000000000, 0.000000000000000000, -1.000000000000000000 ) ) ;
#12015 = EDGE_LOOP ( 'NONE', ( #2295, #2858, #7604, #3694 ) ) ;
#12016 = EDGE_LOOP ( 'NONE', ( #17082, #14738, #8985, #499 ) ) ;
#12017 = CARTESIAN_POINT ( 'NONE',  ( 3.458734125000002546, -1.432654583217639610, 13.12500000136560629 ) ) ;
#12018 = CARTESIAN_POINT ( 'NONE',  ( 52.40625000000000000, 12.99999999999999645, 13.75735931288070191 ) ) ;
#12019 = VECTOR ( 'NONE', #5080, 1000.000000000000000 ) ;
#12020 = EDGE_CURVE ( 'NONE', #7665, #12363, #21407, .T. ) ;
#12021 = CARTESIAN_POINT ( 'NONE',  ( -67.00000000218494733, 9.999999999999998224, 17.49999999999999645 ) ) ;
#12022 = VECTOR ( 'NONE', #19384, 1000.000000000000000 ) ;
#12023 = ADVANCED_FACE ( 'NONE', ( #13419 ), #20685, .T. ) ;
#12024 = DIRECTION ( 'NONE',  ( -0.000000000000000000, -0.000000000000000000, -1.000000000000000000 ) ) ;
#12025 = CARTESIAN_POINT ( 'NONE',  ( -71.74999999999998579, 8.964466094067258695, 17.50000000000000355 ) ) ;
#12026 = DIRECTION ( 'NONE',  ( 0.000000000000000000, 0.000000000000000000, 1.000000000000000000 ) ) ;
#12027 = EDGE_CURVE ( 'NONE', #13738, #7050, #22607, .T. ) ;
#12028 = CARTESIAN_POINT ( 'NONE',  ( 60.71643183416158962, 13.97181229448536399, 16.72490539043799629 ) ) ;
#12029 = CARTESIAN_POINT ( 'NONE',  ( -1.506022603841296270, 0.000000000000000000, -6.735000000000022524 ) ) ;
#12030 = EDGE_CURVE ( 'NONE', #5230, #23216, #8016, .T. ) ;
#12031 = CARTESIAN_POINT ( 'NONE',  ( 3.458734125000000770, 1.432654583217640498, 0.5500000013655963471 ) ) ;
#12032 = CYLINDRICAL_SURFACE ( 'NONE', #3028, 4.000000000000000000 ) ;
#12033 = CARTESIAN_POINT ( 'NONE',  ( 71.70000000000000284, 9.999999999999998224, 17.49999999999999645 ) ) ;
#12034 = CARTESIAN_POINT ( 'NONE',  ( 1.656854249492381470, 4.000000000000000000, 12.81250000273119660 ) ) ;
#12035 = CARTESIAN_POINT ( 'NONE',  ( -68.09999999999999432, 9.999999999999998224, 12.49999999999999289 ) ) ;
#12036 = ORIENTED_EDGE ( 'NONE', *, *, #18486, .T. ) ;
#12037 = DIRECTION ( 'NONE',  ( 0.3420201433256622736, 0.9396926207859106484, 0.000000000000000000 ) ) ;
#12038 = ORIENTED_EDGE ( 'NONE', *, *, #17584, .T. ) ;
#12039 = CARTESIAN_POINT ( 'NONE',  ( 58.46643183416158251, 6.028187705514633343, 13.27509460956200016 ) ) ;
#12040 = CARTESIAN_POINT ( 'NONE',  ( 3.458734125000001214, -1.432654583217639610, 0.1750000013655959863 ) ) ;
#12041 = ORIENTED_EDGE ( 'NONE', *, *, #21928, .F. ) ;
#12042 = FACE_OUTER_BOUND ( 'NONE', #14930, .T. ) ;
#12043 = VERTEX_POINT ( 'NONE', #808 ) ;
#12044 = CARTESIAN_POINT ( 'NONE',  ( -0.9413949561959078505, -0.3373062947069096484, 10.00000000000000888 ) ) ;
#12045 = ORIENTED_EDGE ( 'NONE', *, *, #9040, .F. ) ;
#12046 = PRODUCT ( 'torque nut 08a_iso_ISO 10511-M8-N', 'torque nut 08a_iso_ISO 10511-M8-N', '', ( #13215 ) ) ;
#12047 = CARTESIAN_POINT ( 'NONE',  ( 56.84606816583843880, 8.825410453826357582, 18.02818770551464667 ) ) ;
#12048 = CARTESIAN_POINT ( 'NONE',  ( -67.40000000218495302, 9.999999999999998224, 12.49999999999999289 ) ) ;
#12049 =( BOUNDED_CURVE ( )  B_SPLINE_CURVE ( 2, ( #23123, #17523, #14045, #4933, #10472, #12142, #6850, #21197, #4811 ),
 .UNSPECIFIED., .F., .F. ) 
 B_SPLINE_CURVE_WITH_KNOTS ( ( 3, 2, 2, 2, 3 ),
 ( 0.6500000000000000222, 0.6624999999999999778, 0.6750000000000000444, 0.6875000000000000000, 0.6999999999999999556 ),
 .UNSPECIFIED. ) 
 CURVE ( )  GEOMETRIC_REPRESENTATION_ITEM ( )  RATIONAL_B_SPLINE_CURVE ( ( 1.000000000000000000, 0.9238795325112867385, 1.000000000000000000, 0.9238795325112867385, 1.000000000000000000, 0.9238795325112867385, 1.000000000000000000, 0.9238795325112867385, 1.000000000000000000 ) ) 
 REPRESENTATION_ITEM ( '' )  );
#12050 = EDGE_CURVE ( 'NONE', #12476, #21889, #10060, .T. ) ;
#12051 = CARTESIAN_POINT ( 'NONE',  ( -2.445694354108819635, -2.445694354108820967, -2.887499998634404097 ) ) ;
#12052 = CARTESIAN_POINT ( 'NONE',  ( -19.99999999999999645, -9.000000000000003553, 5.000000000000079936 ) ) ;
#12053 = CARTESIAN_POINT ( 'NONE',  ( 1.025207404391860050E-15, 3.458734125000000770, 19.43750000136560629 ) ) ;
#12054 = CARTESIAN_POINT ( 'NONE',  ( 1.656854249492384135, -3.999999999999999112, 14.43750000273119483 ) ) ;
#12055 = CARTESIAN_POINT ( 'NONE',  ( 57.93750000000000000, 10.00000000000000711, 17.99999999999999645 ) ) ;
#12056 = CARTESIAN_POINT ( 'NONE',  ( 70.50000000109247367, 9.143825827087049163, 17.06698729999999742 ) ) ;
#12057 = EDGE_CURVE ( 'NONE', #13272, #20280, #15572, .T. ) ;
#12058 = CARTESIAN_POINT ( 'NONE',  ( 70.65000000218495302, 11.03553390593268269, 12.49999999999994138 ) ) ;
#12059 = CARTESIAN_POINT ( 'NONE',  ( 57.50231816583843170, 12.07320092032949610, 12.83056023321021044 ) ) ;
#12060 = CARTESIAN_POINT ( 'NONE',  ( 1.432654583217642275, -3.458734124999999882, 2.300000001365597679 ) ) ;
#12061 = CARTESIAN_POINT ( 'NONE',  ( -3.458734124999998993, -1.432654583217642497, 11.75000000136560629 ) ) ;
#12062 = FACE_OUTER_BOUND ( 'NONE', #4357, .T. ) ;
#12063 = CARTESIAN_POINT ( 'NONE',  ( -67.90000000109246514, 10.85617417291294551, 12.93301269999999192 ) ) ;
#12064 = EDGE_LOOP ( 'NONE', ( #20834, #13531, #23284, #10943 ) ) ;
#12065 = CARTESIAN_POINT ( 'NONE',  ( 0.000000000000000000, 9.241976615262133876, 1.699438267350532827 ) ) ;
#12066 = CARTESIAN_POINT ( 'NONE',  ( 65.70000000218495018, 8.232233047033629347, 13.23223304703362402 ) ) ;
#12067 = ORIENTED_EDGE ( 'NONE', *, *, #8201, .T. ) ;
#12068 = LINE ( 'NONE', #4974, #4232 ) ;
#12069 = CIRCLE ( 'NONE', #16251, 4.000000000000000888 ) ;
#12070 = FILL_AREA_STYLE_COLOUR ( '', #11095 ) ;
#12071 = CARTESIAN_POINT ( 'NONE',  ( 2.828427124746190735, -2.828427124746189847, 4.800000002731187543 ) ) ;
#12072 = AXIS2_PLACEMENT_3D ( 'NONE', #22863, #17617, #8280 ) ;
#12073 = ORIENTED_EDGE ( 'NONE', *, *, #16217, .F. ) ;
#12074 = ORIENTED_EDGE ( 'NONE', *, *, #9338, .F. ) ;
#12075 = LINE ( 'NONE', #4627, #22839 ) ;
#12076 = CARTESIAN_POINT ( 'NONE',  ( 36.99310306966726358, -11.25000000000000355, 5.000000000000079936 ) ) ;
#12077 = ORIENTED_EDGE ( 'NONE', *, *, #12789, .F. ) ;
#12078 = CARTESIAN_POINT ( 'NONE',  ( 69.25000000109247367, 9.999999999999998224, 12.93301269999999192 ) ) ;
#12079 = AXIS2_PLACEMENT_3D ( 'NONE', #5444, #21714, #16125 ) ;
#12080 = CARTESIAN_POINT ( 'NONE',  ( 66.85000000109246798, 7.933012699999995476, 14.99999999999999645 ) ) ;
#12081 = AXIS2_PLACEMENT_3D ( 'NONE', #13265, #14826, #11353 ) ;
#12082 = EDGE_CURVE ( 'NONE', #12965, #20008, #23553, .T. ) ;
#12083 = ORIENTED_EDGE ( 'NONE', *, *, #21051, .T. ) ;
#12084 =( BOUNDED_CURVE ( )  B_SPLINE_CURVE ( 2, ( #7594, #14916, #13117, #20019, #1821, #11320, #5544, #2177, #9514 ),
 .UNSPECIFIED., .F., .F. ) 
 B_SPLINE_CURVE_WITH_KNOTS ( ( 3, 2, 2, 2, 3 ),
 ( 0.06249999999999961836, 0.07812499999999952816, 0.09374999999999943101, 0.1093749999999993339, 0.1249999999999992367 ),
 .UNSPECIFIED. ) 
 CURVE ( )  GEOMETRIC_REPRESENTATION_ITEM ( )  RATIONAL_B_SPLINE_CURVE ( ( 1.000000000000001776, 0.9238795325112848511, 1.000000000000000000, 0.9238795325112867385, 1.000000000000000000, 0.9238795325112867385, 1.000000000000000000, 0.9238795325112904022, 0.9999999999999963363 ) ) 
 REPRESENTATION_ITEM ( '' )  );
#12085 = CARTESIAN_POINT ( 'NONE',  ( 0.000000000000000000, 1.239665997527020558, -9.314797388894877628 ) ) ;
#12086 = CARTESIAN_POINT ( 'NONE',  ( 53.06250000000000711, 5.999999999999996447, 15.00000000000001599 ) ) ;
#12087 = CARTESIAN_POINT ( 'NONE',  ( 1.432654583217639832, 3.458734125000000326, 5.425000001365595459 ) ) ;
#12088 = CARTESIAN_POINT ( 'NONE',  ( -2.445694354108818303, -2.445694354108820523, 13.56250000136560629 ) ) ;
#12089 = CARTESIAN_POINT ( 'NONE',  ( 68.00000000218494733, 7.499999999999996447, 14.99999999999999645 ) ) ;
#12090 = DIRECTION ( 'NONE',  ( -0.9396926207859107594, -0.3420201433256623291, 1.540743955509804830E-32 ) ) ;
#12091 = EDGE_LOOP ( 'NONE', ( #14057, #13546, #16856, #8887 ) ) ;
#12092 = DIRECTION ( 'NONE',  ( -0.000000000000000000, -0.000000000000000000, 1.000000000000000000 ) ) ;
#12093 = CARTESIAN_POINT ( 'NONE',  ( 0.000000000000000000, 0.000000000000000000, 3.469446951953614189E-15 ) ) ;
#12094 = PLANE ( 'NONE',  #13503 ) ;
#12095 = VERTEX_POINT ( 'NONE', #14241 ) ;
#12096 = CARTESIAN_POINT ( 'NONE',  ( 2.805705207896068476, -3.226868319750173075, -3.503898532754370354 ) ) ;
#12097 = DIRECTION ( 'NONE',  ( -1.000000000000000000, -0.000000000000000000, -0.000000000000000000 ) ) ;
#12098 = AXIS2_PLACEMENT_3D ( 'NONE', #17389, #19051, #19173 ) ;
#12099 = VECTOR ( 'NONE', #9312, 1000.000000000000000 ) ;
#12100 = LINE ( 'NONE', #12578, #6030 ) ;
#12101 = VERTEX_POINT ( 'NONE', #13995 ) ;
#12102 = CARTESIAN_POINT ( 'NONE',  ( -69.49999999999998579, 7.499999999999996447, 14.99999999999999645 ) ) ;
#12103 = ORIENTED_EDGE ( 'NONE', *, *, #19183, .T. ) ;
#12104 = CARTESIAN_POINT ( 'NONE',  ( 19.99999999999999289, 9.999999999999966249, -20.00000000000000355 ) ) ;
#12105 = FACE_OUTER_BOUND ( 'NONE', #516, .T. ) ;
#12106 = VECTOR ( 'NONE', #103, 1000.000000000000000 ) ;
#12107 = CIRCLE ( 'NONE', #971, 2.499999999999999556 ) ;
#12108 = CARTESIAN_POINT ( 'NONE',  ( -3.250000000000004441, 5.629165124598849879, 0.000000000000000000 ) ) ;
#12109 = CARTESIAN_POINT ( 'NONE',  ( 9.920644283265380691E-16, 4.000000000000000000, 11.75000000000001066 ) ) ;
#12110 = CARTESIAN_POINT ( 'NONE',  ( 67.30000000109247082, 12.06698729999999919, 15.85617417291294196 ) ) ;
#12111 = EDGE_LOOP ( 'NONE', ( #16267, #22096, #19135, #21884, #17508, #21330, #21238 ) ) ;
#12112 = CARTESIAN_POINT ( 'NONE',  ( -15.00000000000000711, -10.00000000000000000, -19.99999999999999645 ) ) ;
#12113 = CARTESIAN_POINT ( 'NONE',  ( 4.000000000000000888, -1.656854249492379694, -1.137499997268811125 ) ) ;
#12114 = CARTESIAN_POINT ( 'NONE',  ( 70.05000000109247082, 7.933012699999995476, 14.99999999999999645 ) ) ;
#12115 = CARTESIAN_POINT ( 'NONE',  ( -2.445694354108818303, -2.445694354108820523, 10.56250000136560452 ) ) ;
#12116 = CARTESIAN_POINT ( 'NONE',  ( -12.44420145928343935, -8.974600000000002353, 5.000000000000079936 ) ) ;
#12117 = CARTESIAN_POINT ( 'NONE',  ( -14.16125006966725053, -11.25000000000000355, 10.00000000000008882 ) ) ;
#12118 = ORIENTED_EDGE ( 'NONE', *, *, #17251, .T. ) ;
#12119 = CARTESIAN_POINT ( 'NONE',  ( -1.656854249492380804, 4.000000000000000000, -2.887499999999997513 ) ) ;
#12120 = CARTESIAN_POINT ( 'NONE',  ( 0.000000000000000000, 0.000000000000000000, -4.694516984716113228 ) ) ;
#12121 = DIRECTION ( 'NONE',  ( 0.000000000000000000, 0.000000000000000000, -1.000000000000000000 ) ) ;
#12122 = CARTESIAN_POINT ( 'NONE',  ( -1.799999999999996048, 7.470345474798879931E-16, 6.000000000000021316 ) ) ;
#12123 = VERTEX_POINT ( 'NONE', #17929 ) ;
#12124 = EDGE_CURVE ( 'NONE', #8828, #15755, #13885, .T. ) ;
#12125 = DIRECTION ( 'NONE',  ( 6.123233995736827666E-17, -1.000000000000000000, 0.000000000000000000 ) ) ;
#12126 = EDGE_LOOP ( 'NONE', ( #17418, #3440, #6132, #11551 ) ) ;
#12127 = CARTESIAN_POINT ( 'NONE',  ( -67.60000000109246798, 7.933012699999995476, 15.85617417291294196 ) ) ;
#12128 = VERTEX_POINT ( 'NONE', #5002 ) ;
#12129 = LINE ( 'NONE', #12489, #10200 ) ;
#12130 = VERTEX_POINT ( 'NONE', #19829 ) ;
#12131 = ORIENTED_EDGE ( 'NONE', *, *, #12812, .F. ) ;
#12132 = CARTESIAN_POINT ( 'NONE',  ( -1.432654583217639166, 3.458734125000000770, 11.50000000136560629 ) ) ;
#12133 = EDGE_CURVE ( 'NONE', #23443, #19414, #8447, .T. ) ;
#12134 = CARTESIAN_POINT ( 'NONE',  ( 2.828427124746189847, 2.828427124746190291, -0.9499999972688126793 ) ) ;
#12135 = CARTESIAN_POINT ( 'NONE',  ( -66.60000000218495586, 9.999999999999998224, 12.49999999999999289 ) ) ;
#12136 = CARTESIAN_POINT ( 'NONE',  ( 66.60000000109248219, 7.933012699999995476, 15.85617417291294196 ) ) ;
#12137 = CARTESIAN_POINT ( 'NONE',  ( -69.45000000000000284, 7.499999999999995559, 16.03553390593273420 ) ) ;
#12138 = DIRECTION ( 'NONE',  ( 0.000000000000000000, 0.000000000000000000, 1.000000000000000000 ) ) ;
#12139 = CARTESIAN_POINT ( 'NONE',  ( 60.00000000000003553, 13.52471821456362910, 16.68728994856221348 ) ) ;
#12140 = VECTOR ( 'NONE', #1558, 1000.000000000000000 ) ;
#12141 = CARTESIAN_POINT ( 'NONE',  ( -1.432654583217641164, -3.458734125000000326, -1.824999998634404097 ) ) ;
#12142 = CARTESIAN_POINT ( 'NONE',  ( -1.656854249492380138, -3.999999999999999112, 13.18750000000001243 ) ) ;
#12143 = CARTESIAN_POINT ( 'NONE',  ( -90.00000000000000000, 0.000000000000000000, -8.073750000000021743 ) ) ;
#12144 = CARTESIAN_POINT ( 'NONE',  ( 2.828427124746192067, -2.828427124746189847, 13.50000000273119660 ) ) ;
#12145 = DIRECTION ( 'NONE',  ( 0.000000000000000000, 0.3090169943749412895, 0.9510565162951556406 ) ) ;
#12146 = EDGE_LOOP ( 'NONE', ( #6834, #16146, #9185, #13860 ) ) ;
#12147 = ADVANCED_FACE ( 'NONE', ( #21143 ), #16147, .T. ) ;
#12148 = CARTESIAN_POINT ( 'NONE',  ( -70.80000000109245661, 9.143825827087052716, 12.93301269999999192 ) ) ;
#12149 = VERTEX_POINT ( 'NONE', #12210 ) ;
#12150 = CARTESIAN_POINT ( 'NONE',  ( 60.06018183416157541, 5.999999999999996447, 14.93194885905437808 ) ) ;
#12151 = CARTESIAN_POINT ( 'NONE',  ( -69.20000000109246230, 9.143825827087050939, 12.93301269999999370 ) ) ;
#12152 = ADVANCED_FACE ( 'NONE', ( #4756 ), #9591, .F. ) ;
#12153 = DIRECTION ( 'NONE',  ( -0.000000000000000000, 1.000000000000000000, -0.000000000000000000 ) ) ;
#12154 = ORIENTED_EDGE ( 'NONE', *, *, #15806, .F. ) ;
#12155 = DIRECTION ( 'NONE',  ( 0.000000000000000000, 0.000000000000000000, -1.000000000000000000 ) ) ;
#12156 = ORIENTED_EDGE ( 'NONE', *, *, #15990, .T. ) ;
#12157 = DIRECTION ( 'NONE',  ( 1.000000000000000000, 0.000000000000000000, 0.000000000000000000 ) ) ;
#12158 = VERTEX_POINT ( 'NONE', #2947 ) ;
#12159 = EDGE_CURVE ( 'NONE', #12128, #15377, #1381, .T. ) ;
#12160 = CARTESIAN_POINT ( 'NONE',  ( 56.37731816583843170, 7.830560233210212218, 12.92679907967049679 ) ) ;
#12161 = CARTESIAN_POINT ( 'NONE',  ( -67.75000000218496155, 11.03553390593273598, 17.50000000000000355 ) ) ;
#12162 = CARTESIAN_POINT ( 'NONE',  ( -60.00000000000000711, 9.999999999999998224, 25.00000000000001421 ) ) ;
#12163 = VECTOR ( 'NONE', #23390, 1000.000000000000000 ) ;
#12164 = CARTESIAN_POINT ( 'NONE',  ( -71.65000000109246514, 7.933012699999995476, 14.99999999999999645 ) ) ;
#12165 = CARTESIAN_POINT ( 'NONE',  ( 2.445694354108822299, -2.445694354108820079, 17.06250000136560629 ) ) ;
#12166 = CARTESIAN_POINT ( 'NONE',  ( 2.828427124746191179, 2.828427124746190291, 12.75000000273119660 ) ) ;
#12167 = CARTESIAN_POINT ( 'NONE',  ( 56.62500000000000000, 12.12132034355964727, 17.12132034355963484 ) ) ;
#12168 = CIRCLE ( 'NONE', #19780, 4.000000000000001776 ) ;
#12169 = DIRECTION ( 'NONE',  ( 0.000000000000000000, 0.000000000000000000, -1.000000000000000000 ) ) ;
#12170 = CIRCLE ( 'NONE', #15617, 11.00000000000000000 ) ;
#12171 = DIRECTION ( 'NONE',  ( 0.000000000000000000, 0.000000000000000000, 1.000000000000000000 ) ) ;
#12172 = CARTESIAN_POINT ( 'NONE',  ( 59.90625000000000711, 12.99999999999999645, 13.75735931288070191 ) ) ;
#12173 = ADVANCED_FACE ( 'NONE', ( #10301 ), #7041, .T. ) ;
#12174 = CARTESIAN_POINT ( 'NONE',  ( 3.458734125000000770, 4.235727675282972223E-16, 3.487500001365597679 ) ) ;
#12175 = CARTESIAN_POINT ( 'NONE',  ( 67.50000000218494733, 11.76776695296636888, 13.23223304703362579 ) ) ;
#12176 = CARTESIAN_POINT ( 'NONE',  ( 67.39999999999999147, 11.76776695296636888, 13.23223304703362579 ) ) ;
#12177 = CARTESIAN_POINT ( 'NONE',  ( -69.65000000109246514, 12.06698730000000097, 14.99999999999999645 ) ) ;
#12178 = ORIENTED_EDGE ( 'NONE', *, *, #270, .F. ) ;
#12179 = DIRECTION ( 'NONE',  ( 1.000000000000000000, 0.000000000000000000, 0.000000000000000000 ) ) ;
#12180 = DIRECTION ( 'NONE',  ( 1.000000000000000000, 0.000000000000000000, 0.000000000000000000 ) ) ;
#12181 = ORIENTED_EDGE ( 'NONE', *, *, #21624, .T. ) ;
#12182 = CARTESIAN_POINT ( 'NONE',  ( 58.96875000000000711, 6.999999999999992895, 13.75735931288071967 ) ) ;
#12183 = APPLICATION_PROTOCOL_DEFINITION ( 'draft international standard', 'automotive_design', 1998, #21378 ) ;
#12184 = CARTESIAN_POINT ( 'NONE',  ( -1.656854249492380804, 4.000000000000000000, 0.2375000027311863493 ) ) ;
#12185 = EDGE_CURVE ( 'NONE', #22332, #19003, #22165, .T. ) ;
#12186 = ORIENTED_EDGE ( 'NONE', *, *, #17156, .T. ) ;
#12187 = ORIENTED_EDGE ( 'NONE', *, *, #1635, .F. ) ;
#12188 = VECTOR ( 'NONE', #1281, 1000.000000000000000 ) ;
#12189 = CARTESIAN_POINT ( 'NONE',  ( -2.000000000000000888, 8.073750000000021743, 0.000000000000000000 ) ) ;
#12190 =( BOUNDED_CURVE ( )  B_SPLINE_CURVE ( 2, ( #11372, #16744, #324, #9579, #203, #13058, #5840, #22467, #9806 ),
 .UNSPECIFIED., .F., .F. ) 
 B_SPLINE_CURVE_WITH_KNOTS ( ( 3, 2, 2, 2, 3 ),
 ( 0.5000000000000000000, 0.5124999999999999556, 0.5250000000000000222, 0.5374999999999999778, 0.5500000000000000444 ),
 .UNSPECIFIED. ) 
 CURVE ( )  GEOMETRIC_REPRESENTATION_ITEM ( )  RATIONAL_B_SPLINE_CURVE ( ( 1.000000000000000000, 0.9238795325112867385, 1.000000000000000000, 0.9238795325112867385, 1.000000000000000000, 0.9238795325112867385, 1.000000000000000000, 0.9238795325112867385, 1.000000000000000000 ) ) 
 REPRESENTATION_ITEM ( '' )  );
#12191 = DIRECTION ( 'NONE',  ( 0.000000000000000000, 0.000000000000000000, 1.000000000000000000 ) ) ;
#12192 = ORIENTED_EDGE ( 'NONE', *, *, #10991, .F. ) ;
#12193 = ADVANCED_FACE ( 'NONE', ( #21620 ), #8495, .T. ) ;
#12194 = PLANE ( 'NONE',  #3777 ) ;
#12195 = AXIS2_PLACEMENT_3D ( 'NONE', #14095, #23415, #4743 ) ;
#12196 = EDGE_CURVE ( 'NONE', #1325, #21072, #22535, .T. ) ;
#12197 = CIRCLE ( 'NONE', #22091, 1.020000000000000018 ) ;
#12198 = CARTESIAN_POINT ( 'NONE',  ( 66.25000000109247367, 12.06698730000000097, 14.99999999999999645 ) ) ;
#12199 = AXIS2_PLACEMENT_3D ( 'NONE', #7368, #18475, #9171 ) ;
#12200 = CARTESIAN_POINT ( 'NONE',  ( 67.55000000109247082, 8.538419263543522320, 16.46158073645647235 ) ) ;
#12201 = CARTESIAN_POINT ( 'NONE',  ( 1.971781867644420635E-15, -4.000000000000000000, 17.37500000273119483 ) ) ;
#12202 = DIRECTION ( 'NONE',  ( 0.000000000000000000, 1.000000000000000000, -1.287488025362403787E-15 ) ) ;
#12203 = CARTESIAN_POINT ( 'NONE',  ( 57.87731816583843170, 7.123453452023657206, 12.21969229848395599 ) ) ;
#12204 = CARTESIAN_POINT ( 'NONE',  ( -3.458734125000000326, 0.000000000000000000, 5.737500001365596347 ) ) ;
#12205 = CARTESIAN_POINT ( 'NONE',  ( -3.458734124999998105, -1.432654583217642275, 16.50000000136560629 ) ) ;
#12206 = DIRECTION ( 'NONE',  ( -0.000000000000000000, -0.000000000000000000, 1.000000000000000000 ) ) ;
#12207 = VECTOR ( 'NONE', #186, 1000.000000000000000 ) ;
#12208 = CARTESIAN_POINT ( 'NONE',  ( -3.999999999999999112, 0.000000000000000000, 12.00000000000001066 ) ) ;
#12209 = EDGE_LOOP ( 'NONE', ( #4424, #11191, #12466, #13836 ) ) ;
#12210 = CARTESIAN_POINT ( 'NONE',  ( -12.45344630323380208, -9.000000000000003553, 10.00000000000008882 ) ) ;
#12211 = COLOUR_RGB ( '', 0.72549020, 0.75294118, 0.79215686) ;
#12212 = CARTESIAN_POINT ( 'NONE',  ( -6.499999999999999112, 2.531211054341943711, -3.440493080744400967 ) ) ;
#12213 = CARTESIAN_POINT ( 'NONE',  ( 7.347880794884118750E-16, -4.000000000000000000, -1.449999999999998179 ) ) ;
#12214 = EDGE_LOOP ( 'NONE', ( #23107, #22591 ) ) ;
#12215 = DIRECTION ( 'NONE',  ( -0.000000000000000000, -1.000000000000000000, -0.000000000000000000 ) ) ;
#12216 = CARTESIAN_POINT ( 'NONE',  ( 4.999999999999999112, -6.478011392632939014, 6.807171995660559638 ) ) ;
#12218 = ADVANCED_FACE ( 'NONE', ( #14713, #9083 ), #69, .F. ) ;
#12217 = AXIS2_PLACEMENT_3D ( 'NONE', #5428, #3514, #7121 ) ;
#12219 = DIRECTION ( 'NONE',  ( 0.3420201433256622736, -0.9396926207859106484, -1.232595164407828100E-31 ) ) ;
#12220 = EDGE_LOOP ( 'NONE', ( #14296, #6284, #5294, #6321 ) ) ;
#12221 = CARTESIAN_POINT ( 'NONE',  ( 65.90000000218495302, 11.76776695296636888, 13.23223304703362579 ) ) ;
#12222 = ORIENTED_EDGE ( 'NONE', *, *, #11193, .T. ) ;
#12223 = EDGE_CURVE ( 'NONE', #17685, #1297, #12910, .T. ) ;
#12224 = VECTOR ( 'NONE', #15647, 1000.000000000000000 ) ;
#12225 = CARTESIAN_POINT ( 'NONE',  ( 58.90856816583844591, 13.97181229448534978, 13.27509460956196641 ) ) ;
#12226 = CARTESIAN_POINT ( 'NONE',  ( 70.20000000218495018, 9.999999999999998224, 17.49999999999999645 ) ) ;
#12227 =( BOUNDED_CURVE ( )  B_SPLINE_CURVE ( 2, ( #3070, #10645, #7031, #6787, #1373, #15791, #17919, #23423, #14464 ),
 .UNSPECIFIED., .F., .F. ) 
 B_SPLINE_CURVE_WITH_KNOTS ( ( 3, 2, 2, 2, 3 ),
 ( 0.9375000000000007772, 0.9531250000000005551, 0.9687500000000004441, 0.9843750000000002220, 1.000000000000000000 ),
 .UNSPECIFIED. ) 
 CURVE ( )  GEOMETRIC_REPRESENTATION_ITEM ( )  RATIONAL_B_SPLINE_CURVE ( ( 0.9999999999999962252, 0.9238795325112905132, 1.000000000000000000, 0.9238795325112867385, 1.000000000000000000, 0.9238795325112867385, 1.000000000000000000, 0.9238795325112867385, 1.000000000000000000 ) ) 
 REPRESENTATION_ITEM ( '' )  );
#12228 = CARTESIAN_POINT ( 'NONE',  ( 71.80000000218494449, 9.999999999999998224, 17.49999999999999645 ) ) ;
#12229 = VECTOR ( 'NONE', #16892, 1000.000000000000000 ) ;
#12230 = CARTESIAN_POINT ( 'NONE',  ( 4.999999999999999112, 0.000000000000000000, 0.000000000000000000 ) ) ;
#12231 = CARTESIAN_POINT ( 'NONE',  ( 66.30000000109247082, 10.85617417291294551, 12.93301269999999192 ) ) ;
#12232 = VERTEX_POINT ( 'NONE', #9431 ) ;
#12233 = APPLICATION_CONTEXT ( 'automotive_design' ) ;
#12234 = CARTESIAN_POINT ( 'NONE',  ( 0.000000000000000000, 5.222868219166856285, 9.680994141368792327 ) ) ;
#12235 = LINE ( 'NONE', #1532, #10323 ) ;
#12236 = AXIS2_PLACEMENT_3D ( 'NONE', #23454, #7062, #21163 ) ;
#12237 = CARTESIAN_POINT ( 'NONE',  ( 66.95000000109246230, 8.538419263543524096, 13.53841926354352054 ) ) ;
#12238 = CARTESIAN_POINT ( 'NONE',  ( -2.445694354108819191, 2.445694354108820523, 18.56250000136560629 ) ) ;
#12239 = LINE ( 'NONE', #22988, #7078 ) ;
#12240 = AXIS2_PLACEMENT_3D ( 'NONE', #7534, #5725, #559 ) ;
#12241 = CARTESIAN_POINT ( 'NONE',  ( 0.000000000000000000, -7.958834565716820464, 7.593217523260554103 ) ) ;
#12242 = ORIENTED_EDGE ( 'NONE', *, *, #8635, .T. ) ;
#12243 = DIRECTION ( 'NONE',  ( 0.000000000000000000, 0.000000000000000000, 1.000000000000000000 ) ) ;
#12244 = CARTESIAN_POINT ( 'NONE',  ( 60.00000000000000711, 12.12132034355963484, 12.87867965644034740 ) ) ;
#12245 = CARTESIAN_POINT ( 'NONE',  ( 27.50000000000000000, 4.500000000000001776, -33.66025403784446723 ) ) ;
#12246 =( NAMED_UNIT ( * ) PLANE_ANGLE_UNIT ( ) SI_UNIT ( $, .RADIAN. ) );
#12247 = ORIENTED_EDGE ( 'NONE', *, *, #8945, .T. ) ;
#12248 = CARTESIAN_POINT ( 'NONE',  ( 6.499999999999999112, -3.752776749732574135, -0.5805565836007695601 ) ) ;
#12249 = CARTESIAN_POINT ( 'NONE',  ( 8.718769219667262149, -11.25000000000000355, 10.00000000000008882 ) ) ;
#12250 = ORIENTED_EDGE ( 'NONE', *, *, #2597, .T. ) ;
#12251 = CYLINDRICAL_SURFACE ( 'NONE', #4048, 4.000000000000001776 ) ;
#12252 = VERTEX_POINT ( 'NONE', #4020 ) ;
#12253 = CARTESIAN_POINT ( 'NONE',  ( -90.00000000000000000, 9.887492094615969966E-16, 8.073750000000021743 ) ) ;
#12254 = ORIENTED_EDGE ( 'NONE', *, *, #23267, .T. ) ;
#12255 = CARTESIAN_POINT ( 'NONE',  ( 3.458734125000002546, -1.432654583217639610, 12.12500000136560629 ) ) ;
#12256 = AXIS2_PLACEMENT_3D ( 'NONE', #3563, #16042, #8735 ) ;
#12257 = CARTESIAN_POINT ( 'NONE',  ( 52.59375000000000711, 11.24264068711927322, 11.99999999999998934 ) ) ;
#12258 = AXIS2_PLACEMENT_3D ( 'NONE', #16956, #291, #6179 ) ;
#12259 = LINE ( 'NONE', #6614, #16342 ) ;
#12260 = CARTESIAN_POINT ( 'NONE',  ( 66.40000000109247935, 10.85617417291294551, 17.06698730000000097 ) ) ;
#12261 = CARTESIAN_POINT ( 'NONE',  ( -1.391697335622809950, -4.043246145443391448, -3.503898532754372575 ) ) ;
#12262 = EDGE_CURVE ( 'NONE', #3750, #11837, #5351, .T. ) ;
#12263 = CARTESIAN_POINT ( 'NONE',  ( -70.39999999999999147, 8.232233047033629347, 13.23223304703362402 ) ) ;
#12264 = AXIS2_PLACEMENT_3D ( 'NONE', #7751, #7631, #5816 ) ;
#12265 = CARTESIAN_POINT ( 'NONE',  ( -19.99999999999999645, -9.000000000000003553, 5.000000000000079936 ) ) ;
#12266 = CARTESIAN_POINT ( 'NONE',  ( 60.00000000000004974, 13.73105986157044001, 13.57812919445311550 ) ) ;
#12267 = CARTESIAN_POINT ( 'NONE',  ( 1.432654583217642275, -3.458734124999999882, 1.300000001365597235 ) ) ;
#12268 = DIRECTION ( 'NONE',  ( 1.000000000000000000, 0.000000000000000000, 0.000000000000000000 ) ) ;
#12269 = FACE_OUTER_BOUND ( 'NONE', #7763, .T. ) ;
#12270 = CARTESIAN_POINT ( 'NONE',  ( -1.432654583217638944, 3.458734125000000326, 18.25000000136560629 ) ) ;
#12271 = CARTESIAN_POINT ( 'NONE',  ( 60.00000000000000000, -10.00000000000000178, 14.99999999999999467 ) ) ;
#12272 = AXIS2_PLACEMENT_3D ( 'NONE', #3980, #22291, #3735 ) ;
#12273 = ORIENTED_EDGE ( 'NONE', *, *, #15438, .F. ) ;
#12274 = DIRECTION ( 'NONE',  ( 0.000000000000000000, -0.000000000000000000, 1.000000000000000000 ) ) ;
#12275 = ORIENTED_EDGE ( 'NONE', *, *, #10434, .T. ) ;
#12276 = CARTESIAN_POINT ( 'NONE',  ( 52.74768183416157541, 7.830560233210222876, 17.07320092032950498 ) ) ;
#12277 = CARTESIAN_POINT ( 'NONE',  ( -66.25000000109247367, 12.06698730000000097, 14.99999999999999645 ) ) ;
#12278 =( NAMED_UNIT ( * ) SI_UNIT ( $, .STERADIAN. ) SOLID_ANGLE_UNIT ( ) );
#12279 = CARTESIAN_POINT ( 'NONE',  ( 3.458734125000000326, 1.432654583217640498, -2.699999998634404541 ) ) ;
#12280 = ORIENTED_EDGE ( 'NONE', *, *, #23535, .F. ) ;
#12281 = VECTOR ( 'NONE', #6187, 1000.000000000000000 ) ;
#12282 = CARTESIAN_POINT ( 'NONE',  ( 14.99999999999995559, 15.00000000000000000, -50.00000000000000000 ) ) ;
#12283 = AXIS2_PLACEMENT_3D ( 'NONE', #4814, #10359, #17649 ) ;
#12284 = ORIENTED_EDGE ( 'NONE', *, *, #21059, .F. ) ;
#12285 = FACE_OUTER_BOUND ( 'NONE', #22273, .T. ) ;
#12286 = ORIENTED_EDGE ( 'NONE', *, *, #6410, .T. ) ;
#12287 = CARTESIAN_POINT ( 'NONE',  ( 55.81481816583843170, 12.99999999999999822, 14.93194885905435676 ) ) ;
#12288 = CARTESIAN_POINT ( 'NONE',  ( -66.50000000218494733, 8.232233047033629347, 13.23223304703362402 ) ) ;
#12289 = CARTESIAN_POINT ( 'NONE',  ( 0.000000000000000000, 0.000000000000000000, -5.000000000000000000 ) ) ;
#12290 = EDGE_CURVE ( 'NONE', #15019, #2372, #9555, .T. ) ;
#12291 = DIRECTION ( 'NONE',  ( -3.393848863725434895E-16, 0.8660254037844414832, 0.4999999999999951705 ) ) ;
#12292 = CARTESIAN_POINT ( 'NONE',  ( -3.458734124999998105, -1.432654583217642497, 16.75000000136560629 ) ) ;
#12293 = ADVANCED_FACE ( 'NONE', ( #11117 ), #12695, .F. ) ;
#12294 = CARTESIAN_POINT ( 'NONE',  ( 4.000000000000000888, -1.656854249492379694, -2.137499997268812013 ) ) ;
#12295 = CARTESIAN_POINT ( 'NONE',  ( 59.71875000000000711, 13.00000000000000711, 16.24264068711927322 ) ) ;
#12296 = AXIS2_PLACEMENT_3D ( 'NONE', #4185, #11397, #5866 ) ;
#12297 = DIRECTION ( 'NONE',  ( 0.000000000000000000, 0.000000000000000000, -1.000000000000000000 ) ) ;
#12298 = CARTESIAN_POINT ( 'NONE',  ( 58.87500000000000711, 7.878679656440349177, 12.87867965644035984 ) ) ;
#12299 = CARTESIAN_POINT ( 'NONE',  ( -2.445694354108820523, 2.445694354108820523, 2.862500001365597235 ) ) ;
#12300 = CARTESIAN_POINT ( 'NONE',  ( -1.722946112685674436, -3.007685260252270787, 2.039999999999996927 ) ) ;
#12301 = EDGE_CURVE ( 'NONE', #14122, #18029, #3112, .T. ) ;
#12302 = LINE ( 'NONE', #10392, #3052 ) ;
#12303 = EDGE_LOOP ( 'NONE', ( #18139, #50, #4028, #7290 ) ) ;
#12304 = CARTESIAN_POINT ( 'NONE',  ( 0.000000000000000000, 0.000000000000000000, 0.000000000000000000 ) ) ;
#12305 = DIRECTION ( 'NONE',  ( 0.000000000000000000, -0.9510565162951566398, 0.3090169943749382919 ) ) ;
#12306 = ORIENTED_EDGE ( 'NONE', *, *, #11048, .T. ) ;
#12307 = CARTESIAN_POINT ( 'NONE',  ( -4.000000000000000000, 0.000000000000000000, -1.574999997268811569 ) ) ;
#12308 = ORIENTED_EDGE ( 'NONE', *, *, #7492, .T. ) ;
#12309 = ORIENTED_EDGE ( 'NONE', *, *, #4387, .F. ) ;
#12310 = CARTESIAN_POINT ( 'NONE',  ( 0.000000000000000000, -9.915734732513254102, 4.762163868918236176 ) ) ;
#12311 = DIRECTION ( 'NONE',  ( 0.000000000000000000, 0.000000000000000000, 1.000000000000000000 ) ) ;
#12312 = ORIENTED_EDGE ( 'NONE', *, *, #13349, .F. ) ;
#12313 = CARTESIAN_POINT ( 'NONE',  ( 68.60000000218495586, 9.999999999999998224, 17.49999999999999645 ) ) ;
#12314 = AXIS2_PLACEMENT_3D ( 'NONE', #5965, #6325, #13763 ) ;
#12315 = CARTESIAN_POINT ( 'NONE',  ( 2.828427124746192067, -2.828427124746189847, 12.37500000000001066 ) ) ;
#12316 = EDGE_CURVE ( 'NONE', #375, #3848, #7159, .T. ) ;
#12317 = VERTEX_POINT ( 'NONE', #21970 ) ;
#12318 = DIRECTION ( 'NONE',  ( 0.000000000000000000, -0.9510565162951566398, 0.3090169943749382919 ) ) ;
#12319 = EDGE_CURVE ( 'NONE', #14904, #10478, #2646, .T. ) ;
#12320 = CARTESIAN_POINT ( 'NONE',  ( 71.74999999999998579, 8.964466094067258695, 17.50000000000000355 ) ) ;
#12321 = ADVANCED_FACE ( 'NONE', ( #13148 ), #12801, .T. ) ;
#12322 = DIRECTION ( 'NONE',  ( -0.3420201433256622181, 0.9396926207859106484, 1.232595164407828100E-31 ) ) ;
#12323 = DIRECTION ( 'NONE',  ( -1.000000000000000000, -0.000000000000000000, 0.000000000000000000 ) ) ;
#12324 = CARTESIAN_POINT ( 'NONE',  ( 57.40856816583844591, 13.97181229448534978, 13.27509460956196641 ) ) ;
#12325 = CARTESIAN_POINT ( 'NONE',  ( 3.458734125000000770, -1.432654583217639610, 4.175000001365593683 ) ) ;
#12326 = EDGE_CURVE ( 'NONE', #6681, #12674, #20173, .T. ) ;
#12327 = CARTESIAN_POINT ( 'NONE',  ( 3.458734125000002102, -1.432654583217639610, 14.87500000136560807 ) ) ;
#12328 = DIRECTION ( 'NONE',  ( 0.000000000000000000, -0.3090169943749349057, -0.9510565162951575280 ) ) ;
#12329 = EDGE_CURVE ( 'NONE', #14633, #2992, #14569, .T. ) ;
#12330 = DIRECTION ( 'NONE',  ( -1.000000000000000000, 0.000000000000000000, 0.000000000000000000 ) ) ;
#12331 = ORIENTED_EDGE ( 'NONE', *, *, #4364, .F. ) ;
#12332 = DIRECTION ( 'NONE',  ( -1.000000000000000000, -0.000000000000000000, -0.000000000000000000 ) ) ;
#12333 =( BOUNDED_CURVE ( )  B_SPLINE_CURVE ( 2, ( #52, #20148, #14693, #7496, #3881, #21949, #5921, #5562, #18491 ),
 .UNSPECIFIED., .F., .F. ) 
 B_SPLINE_CURVE_WITH_KNOTS ( ( 3, 2, 2, 2, 3 ),
 ( 0.8499999999999999778, 0.8625000000000000444, 0.8750000000000000000, 0.8874999999999999556, 0.9000000000000000222 ),
 .UNSPECIFIED. ) 
 CURVE ( )  GEOMETRIC_REPRESENTATION_ITEM ( )  RATIONAL_B_SPLINE_CURVE ( ( 1.000000000000000000, 0.9238795325112867385, 1.000000000000000000, 0.9238795325112867385, 1.000000000000000000, 0.9238795325112867385, 1.000000000000000000, 0.9238795325112867385, 1.000000000000000000 ) ) 
 REPRESENTATION_ITEM ( '' )  );
#12334 = LINE ( 'NONE', #18274, #2884 ) ;
#12335 = CARTESIAN_POINT ( 'NONE',  ( 1.236993788156008760E-15, 0.000000000000000000, -20.00000000000000000 ) ) ;
#12336 = VERTEX_POINT ( 'NONE', #5820 ) ;
#12337 = CARTESIAN_POINT ( 'NONE',  ( 15.00195451966726523, -11.25000000000000355, 10.00000000000008882 ) ) ;
#12338 = CARTESIAN_POINT ( 'NONE',  ( 71.35000000109246798, 8.538419263543522320, 16.46158073645647235 ) ) ;
#12339 = DIRECTION ( 'NONE',  ( 0.000000000000000000, 0.000000000000000000, -1.000000000000000000 ) ) ;
#12340 = ORIENTED_EDGE ( 'NONE', *, *, #18553, .T. ) ;
#12341 = FACE_OUTER_BOUND ( 'NONE', #7436, .T. ) ;
#12342 = ORIENTED_EDGE ( 'NONE', *, *, #5227, .F. ) ;
#12343 = CARTESIAN_POINT ( 'NONE',  ( 57.87731816583843170, 7.123453452023657206, 12.21969229848395599 ) ) ;
#12344 = CARTESIAN_POINT ( 'NONE',  ( 69.25000000218494733, 12.50000000000000000, 16.03553390593273420 ) ) ;
#12345 = CARTESIAN_POINT ( 'NONE',  ( -6.500000000000000000, 3.752776749732564809, -0.5805565836007661185 ) ) ;
#12346 = CARTESIAN_POINT ( 'NONE',  ( -68.49999999999998579, 9.999999999999998224, 17.49999999999999645 ) ) ;
#12347 = EDGE_CURVE ( 'NONE', #3455, #17148, #5740, .T. ) ;
#12348 = CARTESIAN_POINT ( 'NONE',  ( 7.347880794884118750E-16, -4.000000000000000000, -0.4499999999999972911 ) ) ;
#12349 = ORIENTED_EDGE ( 'NONE', *, *, #21634, .F. ) ;
#12350 = CARTESIAN_POINT ( 'NONE',  ( 4.999999999999999112, 7.360373001730986964, -4.729683950898791345 ) ) ;
#12351 = EDGE_CURVE ( 'NONE', #2006, #11365, #22209, .T. ) ;
#12352 = CARTESIAN_POINT ( 'NONE',  ( 4.999999999999999112, 1.239665997526886665, 9.314797388894895391 ) ) ;
#12353 = CARTESIAN_POINT ( 'NONE',  ( 67.50000000109245946, 9.143825827087049163, 17.06698729999999742 ) ) ;
#12354 = CARTESIAN_POINT ( 'NONE',  ( 1.025207404391860050E-15, 3.458734125000000770, 18.43750000136560629 ) ) ;
#12355 = DIRECTION ( 'NONE',  ( -1.000000000000000000, 0.000000000000000000, 0.000000000000000000 ) ) ;
#12356 = EDGE_CURVE ( 'NONE', #2402, #14427, #8819, .T. ) ;
#12357 = CARTESIAN_POINT ( 'NONE',  ( 29.00211400323381028, -9.000000000000003553, 5.000000000000079936 ) ) ;
#12358 = VERTEX_POINT ( 'NONE', #21004 ) ;
#12359 = CARTESIAN_POINT ( 'NONE',  ( -4.000000000000000888, 1.656854249492380804, -1.762499999999997957 ) ) ;
#12360 = CARTESIAN_POINT ( 'NONE',  ( 57.84375000000000711, 8.757359312880723223, 18.00000000000000711 ) ) ;
#12361 = AXIS2_PLACEMENT_3D ( 'NONE', #2834, #460, #12573 ) ;
#12362 = SURFACE_STYLE_FILL_AREA ( #6825 ) ;
#12363 = VERTEX_POINT ( 'NONE', #4492 ) ;
#12364 = CARTESIAN_POINT ( 'NONE',  ( 50.00000000000000000, 10.00000000000001599, 12.50000000000002842 ) ) ;
#12365 = CARTESIAN_POINT ( 'NONE',  ( 1.432654583217639832, 3.458734125000000326, -1.574999998634403875 ) ) ;
#12366 = CYLINDRICAL_SURFACE ( 'NONE', #2081, 8.073750000000021743 ) ;
#12367 = EDGE_LOOP ( 'NONE', ( #3962, #2100, #16732, #21391, #7881 ) ) ;
#12368 = CARTESIAN_POINT ( 'NONE',  ( 50.00000000000000000, 10.00000000000001599, 15.00000000000003020 ) ) ;
#12369 = EDGE_LOOP ( 'NONE', ( #22299, #1724, #7464, #12103, #2424 ) ) ;
#12370 = DIRECTION ( 'NONE',  ( 0.000000000000000000, 0.000000000000000000, -1.000000000000000000 ) ) ;
#12371 = ORIENTED_EDGE ( 'NONE', *, *, #8035, .T. ) ;
#12372 = CARTESIAN_POINT ( 'NONE',  ( -1.432654583217639166, 3.458734125000000770, 14.50000000136560629 ) ) ;
#12373 = CARTESIAN_POINT ( 'NONE',  ( -4.000000000000000000, 0.3987449864459974846, -0.01220643443059782861 ) ) ;
#12374 = CARTESIAN_POINT ( 'NONE',  ( -65.75000000109247367, 8.538419263543522320, 16.46158073645647235 ) ) ;
#12375 = DIRECTION ( 'NONE',  ( 0.000000000000000000, -0.5877852522924802425, 0.8090169943749423442 ) ) ;
#12376 = DIRECTION ( 'NONE',  ( 0.000000000000000000, 0.000000000000000000, 1.000000000000000000 ) ) ;
#12377 = CARTESIAN_POINT ( 'NONE',  ( -69.79999999999999716, 11.76776695296636888, 13.23223304703362579 ) ) ;
#12378 = CARTESIAN_POINT ( 'NONE',  ( 4.999999999999999112, 1.464956435139694646, -10.90201369670496945 ) ) ;
#12379 = EDGE_CURVE ( 'NONE', #16373, #13481, #11834, .T. ) ;
#12380 = CARTESIAN_POINT ( 'NONE',  ( 60.00000000000004974, 12.97738825490581682, 15.73700537498047503 ) ) ;
#12381 = CARTESIAN_POINT ( 'NONE',  ( -2.445694354108819635, -2.445694354108820967, -0.8874999986344025427 ) ) ;
#12382 = DIRECTION ( 'NONE',  ( 1.000000000000000000, 7.703719777548943412E-32, 0.000000000000000000 ) ) ;
#12383 = DIRECTION ( 'NONE',  ( 0.000000000000000000, 0.000000000000000000, -1.000000000000000000 ) ) ;
#12384 = CARTESIAN_POINT ( 'NONE',  ( 2.445694354108821855, -2.445694354108820079, 17.81250000136560274 ) ) ;
#12385 = CARTESIAN_POINT ( 'NONE',  ( -3.729367062499998831, 0.000000000000000000, 19.84375000068280670 ) ) ;
#12386 = ORIENTED_EDGE ( 'NONE', *, *, #3532, .T. ) ;
#12387 = PLANE ( 'NONE',  #13577 ) ;
#12388 = ORIENTED_EDGE ( 'NONE', *, *, #7237, .T. ) ;
#12389 = CARTESIAN_POINT ( 'NONE',  ( 59.87268183416157541, 7.219692298483935566, 12.12345345202367675 ) ) ;
#12390 = CARTESIAN_POINT ( 'NONE',  ( -68.35000000109248219, 8.538419263543524096, 13.53841926354352054 ) ) ;
#12391 = DIRECTION ( 'NONE',  ( 1.000000000000000000, 0.000000000000000000, 0.000000000000000000 ) ) ;
#12392 = CARTESIAN_POINT ( 'NONE',  ( -3.458734125000001214, 0.3674941000104132716, -3.278532042589525908 ) ) ;
#12393 = ORIENTED_EDGE ( 'NONE', *, *, #3972, .T. ) ;
#12394 = CARTESIAN_POINT ( 'NONE',  ( 2.000000000000001776, 0.000000000000000000, 0.000000000000000000 ) ) ;
#12395 = AXIS2_PLACEMENT_3D ( 'NONE', #12065, #13736, #17561 ) ;
#12396 = CIRCLE ( 'NONE', #21134, 6.735000000000022524 ) ;
#12397 = EDGE_LOOP ( 'NONE', ( #9087, #21623, #2576, #13328, #3298 ) ) ;
#12398 = CARTESIAN_POINT ( 'NONE',  ( 34.99999999999999289, 7.500000000000001776, -50.00000000000000000 ) ) ;
#12399 = EDGE_LOOP ( 'NONE', ( #18442, #22588, #18510, #2850, #8851 ) ) ;
#12400 = CARTESIAN_POINT ( 'NONE',  ( 58.81481816583843170, 12.99999999999999822, 14.93194885905435676 ) ) ;
#12401 = CARTESIAN_POINT ( 'NONE',  ( -68.15000000218495302, 8.964466094067258695, 12.49999999999999289 ) ) ;
#12402 = CARTESIAN_POINT ( 'NONE',  ( -0.8800590352214046064, 5.420839058164813373, -26.84672628368516811 ) ) ;
#12403 = DIRECTION ( 'NONE',  ( 0.3420201433256622181, 0.9396926207859107594, -6.162975822039141593E-32 ) ) ;
#12404 = CARTESIAN_POINT ( 'NONE',  ( -3.458734124999999437, 0.000000000000000000, 14.68750000136560452 ) ) ;
#12405 = CARTESIAN_POINT ( 'NONE',  ( -65.00000000000000000, -10.00000000000000178, 14.99999999999999467 ) ) ;
#12406 = CARTESIAN_POINT ( 'NONE',  ( 59.90625000000000711, 12.99999999999999645, 13.75735931288070191 ) ) ;
#12407 = CYLINDRICAL_SURFACE ( 'NONE', #20149, 2.649999999999992806 ) ;
#12408 = CARTESIAN_POINT ( 'NONE',  ( 50.56481816583844591, 6.999999999999998224, 15.06805114094563436 ) ) ;
#12409 = CARTESIAN_POINT ( 'NONE',  ( 2.445694354108820967, -2.445694354108820079, 0.3625000013655968467 ) ) ;
#12410 = DIRECTION ( 'NONE',  ( 1.000000000000000000, 7.703719777548943412E-32, 0.000000000000000000 ) ) ;
#12411 = CARTESIAN_POINT ( 'NONE',  ( 70.35000000218495586, 7.499999999999996447, 16.03553390593273775 ) ) ;
#12412 = ORIENTED_EDGE ( 'NONE', *, *, #547, .T. ) ;
#12413 = LINE ( 'NONE', #19679, #5625 ) ;
#12414 = CARTESIAN_POINT ( 'NONE',  ( -2.117863837641483646E-16, 3.458734125000000770, -3.295601554149324208 ) ) ;
#12415 = ORIENTED_EDGE ( 'NONE', *, *, #20746, .F. ) ;
#12416 = DIRECTION ( 'NONE',  ( 0.000000000000000000, 0.000000000000000000, -1.000000000000000000 ) ) ;
#12417 =( NAMED_UNIT ( * ) PLANE_ANGLE_UNIT ( ) SI_UNIT ( $, .RADIAN. ) );
#12418 = CARTESIAN_POINT ( 'NONE',  ( -4.000000000000000888, 1.656854249492380804, 0.3625000027311864881 ) ) ;
#12419 = DIRECTION ( 'NONE',  ( -1.000000000000000000, -0.000000000000000000, 0.000000000000000000 ) ) ;
#12420 = ORIENTED_EDGE ( 'NONE', *, *, #8932, .F. ) ;
#12421 = ORIENTED_EDGE ( 'NONE', *, *, #7237, .F. ) ;
#12422 = EDGE_CURVE ( 'NONE', #15525, #12867, #4623, .T. ) ;
#12423 = DIRECTION ( 'NONE',  ( -1.000000000000000000, 0.000000000000000000, 1.224646799147353207E-16 ) ) ;
#12424 = AXIS2_PLACEMENT_3D ( 'NONE', #6914, #8592, #8711 ) ;
#12425 = EDGE_CURVE ( 'NONE', #13738, #6569, #788, .T. ) ;
#12426 = DIRECTION ( 'NONE',  ( 0.000000000000000000, 0.000000000000000000, 1.000000000000000000 ) ) ;
#12427 = ORIENTED_EDGE ( 'NONE', *, *, #14956, .T. ) ;
#12428 = SURFACE_STYLE_FILL_AREA ( #14097 ) ;
#12429 = DIRECTION ( 'NONE',  ( -1.000000000000000000, 0.000000000000000000, 0.000000000000000000 ) ) ;
#12430 = ORIENTED_EDGE ( 'NONE', *, *, #5031, .F. ) ;
#12431 = EDGE_CURVE ( 'NONE', #5121, #3084, #20533, .T. ) ;
#12432 = CARTESIAN_POINT ( 'NONE',  ( 66.35000000109248219, 11.46158073645647235, 16.46158073645647235 ) ) ;
#12433 = CARTESIAN_POINT ( 'NONE',  ( 71.20000000000000284, 8.232233047033629347, 13.23223304703362402 ) ) ;
#12434 = DIRECTION ( 'NONE',  ( -1.000000000000000000, 0.000000000000000000, 0.000000000000000000 ) ) ;
#12435 = CARTESIAN_POINT ( 'NONE',  ( 69.45000000000000284, 7.499999999999996447, 16.03553390593273775 ) ) ;
#12436 = CARTESIAN_POINT ( 'NONE',  ( 52.87500000000000711, 7.171572875253794166, 12.17157287525381726 ) ) ;
#12437 = CARTESIAN_POINT ( 'NONE',  ( -1.432654583217640276, 3.458734125000000326, 5.550000001365596347 ) ) ;
#12438 = FILL_AREA_STYLE_COLOUR ( '', #5333 ) ;
#12439 = CARTESIAN_POINT ( 'NONE',  ( -1.432654583217639610, -3.458734124999999882, 15.62500000136560629 ) ) ;
#12440 = CARTESIAN_POINT ( 'NONE',  ( 1.971781867644420635E-15, -4.000000000000000000, 18.37500000273119483 ) ) ;
#12441 = LINE ( 'NONE', #3188, #14388 ) ;
#12442 = ORIENTED_EDGE ( 'NONE', *, *, #546, .T. ) ;
#12443 = CARTESIAN_POINT ( 'NONE',  ( 2.499999999999999556, -10.82112760146734765, -1.975651141462352767 ) ) ;
#12444 = FACE_BOUND ( 'NONE', #15563, .T. ) ;
#12445 = DIRECTION ( 'NONE',  ( -1.000000000000000000, 0.000000000000000000, -0.000000000000000000 ) ) ;
#12446 = ORIENTED_EDGE ( 'NONE', *, *, #18793, .T. ) ;
#12447 = EDGE_CURVE ( 'NONE', #14331, #16324, #22225, .T. ) ;
#12448 = CARTESIAN_POINT ( 'NONE',  ( -60.00000000000000711, 15.00000000000000000, 20.00000000000001421 ) ) ;
#12449 = CARTESIAN_POINT ( 'NONE',  ( 0.000000000000000000, -9.241976615262169403, 1.699438267350339871 ) ) ;
#12450 = EDGE_CURVE ( 'NONE', #10374, #13219, #13104, .T. ) ;
#12451 = EDGE_LOOP ( 'NONE', ( #3134, #15522, #8059, #9239, #19224 ) ) ;
#12452 = FACE_OUTER_BOUND ( 'NONE', #5053, .T. ) ;
#12453 = VERTEX_POINT ( 'NONE', #19108 ) ;
#12454 = DIRECTION ( 'NONE',  ( 0.3420201433256622181, 0.9396926207859107594, -6.162975822039141593E-32 ) ) ;
#12455 = ORIENTED_EDGE ( 'NONE', *, *, #20930, .F. ) ;
#12456 = CIRCLE ( 'NONE', #14743, 4.000000000000000000 ) ;
#12457 = CARTESIAN_POINT ( 'NONE',  ( 55.03125000000000000, 11.65685424949239923, 18.99999999999998934 ) ) ;
#12458 = AXIS2_PLACEMENT_3D ( 'NONE', #12726, #11266, #16410 ) ;
#12459 = CIRCLE ( 'NONE', #12072, 4.000000000000002665 ) ;
#12460 = ADVANCED_FACE ( 'NONE', ( #7754 ), #18757, .T. ) ;
#12461 = CARTESIAN_POINT ( 'NONE',  ( 67.45000000218493597, 11.03553390593273598, 12.49999999999999289 ) ) ;
#12462 = EDGE_CURVE ( 'NONE', #22180, #19202, #14947, .T. ) ;
#12463 = CARTESIAN_POINT ( 'NONE',  ( 0.000000000000000000, 0.000000000000000000, 0.000000000000000000 ) ) ;
#12464 = DIRECTION ( 'NONE',  ( -1.000000000000000000, -7.703719777548943412E-32, 0.000000000000000000 ) ) ;
#12465 = CARTESIAN_POINT ( 'NONE',  ( 1.656854249492383024, -3.999999999999999112, -0.3874999999999968470 ) ) ;
#12466 = ORIENTED_EDGE ( 'NONE', *, *, #12662, .F. ) ;
#12467 = LINE ( 'NONE', #21878, #19097 ) ;
#12468 =( BOUNDED_CURVE ( )  B_SPLINE_CURVE ( 2, ( #21955, #16709, #2202, #11345, #14699, #23658, #5928, #7272, #22067, #13136, #16835, #2078, #9542, #5453, #14941, #7502, #5685, #414, #13257, #7743, #20283, #3763, #9418, #22196, #18260, #12788, #3885, #18383, #1845, #58, #1963, #20042, #10981, #12897, #5809, #15058, #13022, #14818, #9194, #11219, #20399, #5569, #20519, #4122, #16478, #22314, #16593, #11466, #18742, #7390, #20155, #11103, #15644, #4475, #2906, #22675, #642, #7850, #15175, #18968, #11584, #769, #2550, #13603, #2438, #22917, #17069, #6286, #17429, #22433, #8322, #9896, #4360, #2684, #11698, #6045, #8102, #17311, #11942, #21103, #12051, #10023, #6529, #20868, #22794, #10136, #15413 ),
 .UNSPECIFIED., .F., .F. ) 
 B_SPLINE_CURVE_WITH_KNOTS ( ( 3, 2, 2, 2, 2, 2, 2, 2, 2, 2, 2, 2, 2, 2, 2, 2, 2, 2, 2, 2, 2, 2, 2, 2, 2, 2, 2, 2, 2, 2, 2, 2, 2, 2, 2, 2, 2, 2, 2, 2, 2, 2, 2, 3 ),
 ( 0.3947128431780269620, 0.4000000000000000222, 0.4124999999999999778, 0.4249999999999999889, 0.4375000000000000000, 0.4500000000000000111, 0.4625000000000000222, 0.4749999999999999778, 0.4874999999999999889, 0.5000000000000000000, 0.5124999999999999556, 0.5250000000000000222, 0.5374999999999999778, 0.5500000000000000444, 0.5625000000000000000, 0.5749999999999999556, 0.5875000000000000222, 0.5999999999999999778, 0.6125000000000000444, 0.6250000000000000000, 0.6374999999999999556, 0.6500000000000000222, 0.6624999999999999778, 0.6750000000000000444, 0.6875000000000000000, 0.6999999999999999556, 0.7125000000000000222, 0.7249999999999999778, 0.7375000000000000444, 0.7500000000000000000, 0.7624999999999999556, 0.7750000000000000222, 0.7874999999999999778, 0.8000000000000000444, 0.8125000000000000000, 0.8249999999999999556, 0.8375000000000000222, 0.8499999999999999778, 0.8625000000000000444, 0.8750000000000000000, 0.8874999999999999556, 0.8999999999999999112, 0.9124999999999998668, 0.9250000000000000444 ),
 .UNSPECIFIED. ) 
 CURVE ( )  GEOMETRIC_REPRESENTATION_ITEM ( )  RATIONAL_B_SPLINE_CURVE ( ( 0.9628430465414361539, 0.9678031320820217331, 1.000000000000000000, 0.9238795325112867385, 1.000000000000000000, 0.9238795325112867385, 1.000000000000000000, 0.9238795325112867385, 1.000000000000000000, 0.9238795325112867385, 1.000000000000000000, 0.9238795325112867385, 1.000000000000000000, 0.9238795325112867385, 1.000000000000000000, 0.9238795325112867385, 1.000000000000000000, 0.9238795325112867385, 1.000000000000000000, 0.9238795325112867385, 1.000000000000000000, 0.9238795325112867385, 1.000000000000000000, 0.9238795325112867385, 1.000000000000000000, 0.9238795325112867385, 1.000000000000000000, 0.9238795325112867385, 1.000000000000000000, 0.9238795325112867385, 1.000000000000000000, 0.9238795325112867385, 1.000000000000000000, 0.9238795325112867385, 1.000000000000000000, 0.9238795325112867385, 1.000000000000000000, 0.9238795325112867385, 1.000000000000000000, 0.9238795325112867385, 1.000000000000000000, 0.9238795325112867385, 1.000000000000000000, 0.9238795325112867385, 1.000000000000000000, 0.9238795325112867385, 1.000000000000000000, 0.9238795325112867385, 1.000000000000000000, 0.9238795325112867385, 1.000000000000000000, 0.9238795325112867385, 1.000000000000000000, 0.9238795325112867385, 1.000000000000000000, 0.9238795325112867385, 1.000000000000000000, 0.9238795325112867385, 1.000000000000000000, 0.9238795325112867385, 1.000000000000000000, 0.9238795325112867385, 1.000000000000000000, 0.9238795325112867385, 1.000000000000000000, 0.9238795325112867385, 1.000000000000000000, 0.9238795325112867385, 1.000000000000000000, 0.9238795325112867385, 1.000000000000000000, 0.9238795325112867385, 1.000000000000000000, 0.9238795325112867385, 1.000000000000000000, 0.9238795325112867385, 1.000000000000000000, 0.9238795325112867385, 1.000000000000000000, 0.9238795325112867385, 1.000000000000000000, 0.9238795325112867385, 1.000000000000000000, 0.9238795325112867385, 1.000000000000000000, 0.9238795325112867385, 1.000000000000000000 ) ) 
 REPRESENTATION_ITEM ( '' )  );
#12469 = CARTESIAN_POINT ( 'NONE',  ( 58.93518183416157541, 9.931948859054379852, 18.99999999999999289 ) ) ;
#12470 = DIRECTION ( 'NONE',  ( 0.3420201433256622736, 0.9396926207859106484, 0.000000000000000000 ) ) ;
#12471 = CARTESIAN_POINT ( 'NONE',  ( 67.15000000109247935, 11.46158073645647235, 13.53841926354352232 ) ) ;
#12472 = CARTESIAN_POINT ( 'NONE',  ( -3.458734124999999437, 0.000000000000000000, 17.68750000136560274 ) ) ;
#12473 = DIRECTION ( 'NONE',  ( -1.000000000000000000, -0.000000000000000000, 0.000000000000000000 ) ) ;
#12474 = AXIS2_PLACEMENT_3D ( 'NONE', #1691, #14302, #19778 ) ;
#12475 = CARTESIAN_POINT ( 'NONE',  ( 4.999999999999999112, -9.314797388894882957, -1.239665997526988139 ) ) ;
#12476 = VERTEX_POINT ( 'NONE', #15429 ) ;
#12477 = DIRECTION ( 'NONE',  ( 0.000000000000000000, 0.000000000000000000, 1.000000000000000000 ) ) ;
#12478 = CARTESIAN_POINT ( 'NONE',  ( 58.31250000000000000, 13.00000000000000000, 14.99999999999998757 ) ) ;
#12479 = ADVANCED_FACE ( 'NONE', ( #13268 ), #15555, .F. ) ;
#12480 = CIRCLE ( 'NONE', #10171, 4.000000000000000888 ) ;
#12481 = CARTESIAN_POINT ( 'NONE',  ( 1.656854249492383024, -3.999999999999999112, 0.7375000027311867656 ) ) ;
#12482 = LINE ( 'NONE', #18078, #7265 ) ;
#12483 = ORIENTED_EDGE ( 'NONE', *, *, #20495, .F. ) ;
#12484 = DIRECTION ( 'NONE',  ( -1.000000000000000000, 0.000000000000000000, 0.000000000000000000 ) ) ;
#12485 = CARTESIAN_POINT ( 'NONE',  ( 1.432654583217642275, -3.458734124999999437, -2.949999998634404985 ) ) ;
#12486 = DIRECTION ( 'NONE',  ( 1.000000000000000000, -0.000000000000000000, -0.000000000000000000 ) ) ;
#12487 = ADVANCED_FACE ( 'NONE', ( #13622 ), #22583, .F. ) ;
#12488 = ORIENTED_EDGE ( 'NONE', *, *, #9943, .F. ) ;
#12489 = CARTESIAN_POINT ( 'NONE',  ( 19.99999999999999289, 9.999999999999964473, -20.00000000000000355 ) ) ;
#12490 = ORIENTED_EDGE ( 'NONE', *, *, #1794, .F. ) ;
#12491 = VECTOR ( 'NONE', #11894, 1000.000000000000114 ) ;
#12492 = DIRECTION ( 'NONE',  ( -1.000000000000000000, 0.000000000000000000, -0.000000000000000000 ) ) ;
#12493 = ORIENTED_EDGE ( 'NONE', *, *, #7622, .T. ) ;
#12494 = CARTESIAN_POINT ( 'NONE',  ( 4.000000000000001776, -1.656854249492379694, 19.43750000000001066 ) ) ;
#12495 = EDGE_CURVE ( 'NONE', #6076, #18376, #23285, .T. ) ;
#12496 = DIRECTION ( 'NONE',  ( -1.000000000000000000, 0.000000000000000000, -0.000000000000000000 ) ) ;
#12497 = ADVANCED_FACE ( 'NONE', ( #3050 ), #16121, .F. ) ;
#12498 = VECTOR ( 'NONE', #18822, 1000.000000000000000 ) ;
#12499 = DIRECTION ( 'NONE',  ( 0.000000000000000000, 0.9510565162951545304, -0.3090169943749446757 ) ) ;
#12500 = AXIS2_PLACEMENT_3D ( 'NONE', #10653, #3546, #23668 ) ;
#12501 = PRESENTATION_STYLE_ASSIGNMENT (( #7338 ) ) ;
#12502 = CARTESIAN_POINT ( 'NONE',  ( -6.473970235329672780E-16, -4.862606272033106691, -3.745885042887442395 ) ) ;
#12503 = CARTESIAN_POINT ( 'NONE',  ( -71.20000000000000284, 8.232233047033629347, 13.23223304703362402 ) ) ;
#12504 = LINE ( 'NONE', #12265, #18743 ) ;
#12505 = CARTESIAN_POINT ( 'NONE',  ( 60.00000000000002842, 13.86373736226824427, 15.83363142472004448 ) ) ;
#12506 = CARTESIAN_POINT ( 'NONE',  ( 1.432654583217640276, 3.458734125000000770, -0.3249999986344045411 ) ) ;
#12507 = LINE ( 'NONE', #17988, #2639 ) ;
#12508 = LINE ( 'NONE', #21436, #11910 ) ;
#12509 = CARTESIAN_POINT ( 'NONE',  ( 3.458734125000001214, 4.235727675282971730E-16, 17.93750000136560274 ) ) ;
#12510 = CYLINDRICAL_SURFACE ( 'NONE', #22168, 4.000000000000001776 ) ;
#12511 = ORIENTED_EDGE ( 'NONE', *, *, #10837, .F. ) ;
#12512 = CARTESIAN_POINT ( 'NONE',  ( -71.90000000109247935, 12.06698729999999919, 15.85617417291294196 ) ) ;
#12513 = EDGE_LOOP ( 'NONE', ( #14814, #5588, #12548, #17204 ) ) ;
#12514 = CARTESIAN_POINT ( 'NONE',  ( 55.18518183416157541, 10.06805114094561659, 10.99999999999999645 ) ) ;
#12515 = CARTESIAN_POINT ( 'NONE',  ( -68.85000000109248219, 9.999999999999998224, 17.06698730000000097 ) ) ;
#12516 =( NAMED_UNIT ( * ) SI_UNIT ( $, .STERADIAN. ) SOLID_ANGLE_UNIT ( ) );
#12517 = CARTESIAN_POINT ( 'NONE',  ( 3.458734125000000326, 1.432654583217640498, -1.699999998634403875 ) ) ;
#12518 = ORIENTED_EDGE ( 'NONE', *, *, #12462, .T. ) ;
#12519 = DIRECTION ( 'NONE',  ( 0.3420201433256622736, 0.9396926207859106484, 0.000000000000000000 ) ) ;
#12520 = VERTEX_POINT ( 'NONE', #4738 ) ;
#12521 = CARTESIAN_POINT ( 'NONE',  ( 0.000000000000000000, 0.000000000000000000, 1.734723475976807094E-15 ) ) ;
#12522 = ORIENTED_EDGE ( 'NONE', *, *, #23233, .T. ) ;
#12523 = EDGE_CURVE ( 'NONE', #2255, #14480, #17216, .T. ) ;
#12524 = CARTESIAN_POINT ( 'NONE',  ( 50.18981816583844591, 9.931948859054354983, 11.99999999999999645 ) ) ;
#12525 = ADVANCED_FACE ( 'NONE', ( #3407 ), #13864, .T. ) ;
#12526 = CARTESIAN_POINT ( 'NONE',  ( -68.70000000218495018, 8.232233047033627571, 16.76776695296636532 ) ) ;
#12527 = CARTESIAN_POINT ( 'NONE',  ( 0.000000000000000000, -4.729683950898921907, 7.360373001730902587 ) ) ;
#12528 = CARTESIAN_POINT ( 'NONE',  ( -72.10000000109246798, 12.06698730000000275, 15.85617417291294196 ) ) ;
#12529 = CARTESIAN_POINT ( 'NONE',  ( -2.445694354108818303, -2.445694354108820967, 13.81250000136560629 ) ) ;
#12530 = CARTESIAN_POINT ( 'NONE',  ( 4.000000000000000888, 4.898587196589412829E-16, 11.62500000273119660 ) ) ;
#12531 = CARTESIAN_POINT ( 'NONE',  ( 58.40625000000000711, 12.99999999999999645, 13.75735931288070191 ) ) ;
#12532 = FACE_OUTER_BOUND ( 'NONE', #954, .T. ) ;
#12533 = CARTESIAN_POINT ( 'NONE',  ( 57.56250000000000000, 6.999999999999997335, 15.00000000000000533 ) ) ;
#12534 = CARTESIAN_POINT ( 'NONE',  ( -3.999999999999999112, 0.000000000000000000, 19.12500000273119838 ) ) ;
#12535 = CARTESIAN_POINT ( 'NONE',  ( -1.656854249492380138, -3.999999999999999112, 18.31250000273119838 ) ) ;
#12536 = DIRECTION ( 'NONE',  ( -1.000000000000000000, -0.000000000000000000, -0.000000000000000000 ) ) ;
#12537 = AXIS2_PLACEMENT_3D ( 'NONE', #20122, #18118, #1813 ) ;
#12538 = ORIENTED_EDGE ( 'NONE', *, *, #5455, .F. ) ;
#12539 = CARTESIAN_POINT ( 'NONE',  ( -4.000000000000000000, -0.3979232138631226823, -3.896351557369779711E-17 ) ) ;
#12540 = CARTESIAN_POINT ( 'NONE',  ( 4.999999999999999112, -7.360373001730883935, -4.729683950898952105 ) ) ;
#12541 = ORIENTED_EDGE ( 'NONE', *, *, #11725, .T. ) ;
#12542 = CARTESIAN_POINT ( 'NONE',  ( 57.28125000000000711, 8.757359312880703683, 11.99999999999999822 ) ) ;
#12543 = SHAPE_DEFINITION_REPRESENTATION ( #15678, #8403 ) ;
#12544 = CARTESIAN_POINT ( 'NONE',  ( 4.000000000000000888, -1.656854249492379694, -0.1374999972688120964 ) ) ;
#12545 = LINE ( 'NONE', #3527, #3242 ) ;
#12546 = VERTEX_POINT ( 'NONE', #2923 ) ;
#12547 = CARTESIAN_POINT ( 'NONE',  ( -2.828427124746189403, 2.828427124746190291, 17.87500000000001066 ) ) ;
#12548 = ORIENTED_EDGE ( 'NONE', *, *, #5227, .T. ) ;
#12549 = FILL_AREA_STYLE ('',( #10635 ) ) ;
#12550 = CIRCLE ( 'NONE', #16333, 4.000000000000001776 ) ;
#12551 = FACE_OUTER_BOUND ( 'NONE', #13809, .T. ) ;
#12552 = ORIENTED_EDGE ( 'NONE', *, *, #19741, .T. ) ;
#12553 = AXIS2_PLACEMENT_3D ( 'NONE', #3644, #18495, #9660 ) ;
#12554 = LINE ( 'NONE', #3419, #7943 ) ;
#12555 = ORIENTED_EDGE ( 'NONE', *, *, #12422, .T. ) ;
#12556 = LINE ( 'NONE', #10763, #15612 ) ;
#12557 = AXIS2_PLACEMENT_3D ( 'NONE', #12189, #16006, #15891 ) ;
#12558 = VECTOR ( 'NONE', #5452, 1000.000000000000000 ) ;
#12559 = CARTESIAN_POINT ( 'NONE',  ( 72.50000000000000000, 9.999999999999998224, 17.49999999999999645 ) ) ;
#12560 = CARTESIAN_POINT ( 'NONE',  ( 4.000000000000001776, -1.656854249492379694, 17.56250000273119483 ) ) ;
#12561 = EDGE_CURVE ( 'NONE', #21784, #7680, #12068, .T. ) ;
#12562 = CARTESIAN_POINT ( 'NONE',  ( 69.70000000000000284, 9.999999999999998224, 12.49999999999999289 ) ) ;
#12563 = CARTESIAN_POINT ( 'NONE',  ( 51.28125000000000000, 8.343145750507600766, 11.00000000000000533 ) ) ;
#12564 = CARTESIAN_POINT ( 'NONE',  ( 6.353591512924457348E-16, -3.458734125000000326, 2.987500001365597235 ) ) ;
#12565 = SURFACE_STYLE_FILL_AREA ( #5220 ) ;
#12566 = CARTESIAN_POINT ( 'NONE',  ( 1.432654583217641164, 3.458734125000000326, 16.12500000136560629 ) ) ;
#12567 = CARTESIAN_POINT ( 'NONE',  ( 2.499999999999999556, -5.222868219166784343, -9.680994141368829631 ) ) ;
#12568 = AXIS2_PLACEMENT_3D ( 'NONE', #19848, #16391, #20074 ) ;
#12569 = DIRECTION ( 'NONE',  ( -1.000000000000000000, 0.000000000000000000, -0.000000000000000000 ) ) ;
#12570 = VERTEX_POINT ( 'NONE', #19454 ) ;
#12571 = DIRECTION ( 'NONE',  ( 0.000000000000000000, 0.000000000000000000, 1.000000000000000000 ) ) ;
#12572 = CARTESIAN_POINT ( 'NONE',  ( 19.99999999999999645, 4.500000000000003553, -50.00000000000000000 ) ) ;
#12573 = DIRECTION ( 'NONE',  ( 0.000000000000000000, 0.000000000000000000, -1.000000000000000000 ) ) ;
#12574 = ORIENTED_EDGE ( 'NONE', *, *, #1907, .T. ) ;
#12575 = CIRCLE ( 'NONE', #2203, 9.000000000000000000 ) ;
#12576 = ORIENTED_EDGE ( 'NONE', *, *, #14917, .T. ) ;
#12577 = DIRECTION ( 'NONE',  ( -3.081487911019570796E-32, -0.3420201433256691015, 0.9396926207859083169 ) ) ;
#12578 = CARTESIAN_POINT ( 'NONE',  ( -5.007715329123867711E-16, -7.505553499465146494, -3.700000000000000178 ) ) ;
#12579 = VERTEX_POINT ( 'NONE', #17905 ) ;
#12580 = CARTESIAN_POINT ( 'NONE',  ( -27.50000000000000711, 4.500000000000001776, -33.66025403784446723 ) ) ;
#12581 = ORIENTED_EDGE ( 'NONE', *, *, #3662, .F. ) ;
#12582 = CARTESIAN_POINT ( 'NONE',  ( 51.84375000000001421, 8.343145750507638070, 19.00000000000000711 ) ) ;
#12583 = CARTESIAN_POINT ( 'NONE',  ( 67.20000000218495018, 7.499999999999996447, 14.99999999999999645 ) ) ;
#12584 = COLOUR_RGB ( '', 0.08235294, 0.09019608, 0.10196078) ;
#12585 = PLANE ( 'NONE',  #2268 ) ;
#12586 = CARTESIAN_POINT ( 'NONE',  ( 0.000000000000000000, 0.000000000000000000, 0.000000000000000000 ) ) ;
#12587 = CARTESIAN_POINT ( 'NONE',  ( 38.41764710928345750, -8.974600000000002353, 5.000000000000079936 ) ) ;
#12588 = ORIENTED_EDGE ( 'NONE', *, *, #15956, .F. ) ;
#12589 = CARTESIAN_POINT ( 'NONE',  ( 2.828427124746192067, -2.828427124746189847, 17.50000000273119483 ) ) ;
#12590 = AXIS2_PLACEMENT_3D ( 'NONE', #1839, #3640, #7142 ) ;
#12591 = ADVANCED_FACE ( 'NONE', ( #21120 ), #19777, .T. ) ;
#12592 = CIRCLE ( 'NONE', #2951, 6.735000000000022524 ) ;
#12593 = CARTESIAN_POINT ( 'NONE',  ( -0.6937372685066653943, 4.453844082567723461, -3.610536846335889116 ) ) ;
#12594 = EDGE_CURVE ( 'NONE', #16416, #12095, #4685, .T. ) ;
#12595 = CARTESIAN_POINT ( 'NONE',  ( 58.18518183416157541, 10.06805114094561659, 10.99999999999999645 ) ) ;
#12596 = CARTESIAN_POINT ( 'NONE',  ( 13.28490590928345405, -8.974600000000002353, 5.000000000000079936 ) ) ;
#12597 = CARTESIAN_POINT ( 'NONE',  ( 66.30000000109247082, 10.85617417291294551, 12.93301269999999370 ) ) ;
#12598 = CARTESIAN_POINT ( 'NONE',  ( -1.067197363239236640, -6.889406814520513400, -0.2573354458087871444 ) ) ;
#12599 = CARTESIAN_POINT ( 'NONE',  ( -19.99999999999999645, -15.00000000000001954, 10.00000000000008882 ) ) ;
#12600 = VERTEX_POINT ( 'NONE', #19285 ) ;
#12601 = CARTESIAN_POINT ( 'NONE',  ( -0.1973187206307981389, 3.458734125000000326, -3.295601554149323764 ) ) ;
#12602 = CARTESIAN_POINT ( 'NONE',  ( 54.93750000000000711, 10.00000000000000711, 17.99999999999999645 ) ) ;
#12603 = CARTESIAN_POINT ( 'NONE',  ( 0.000000000000000000, 0.000000000000000000, 2.039999999999998259 ) ) ;
#12604 = EDGE_CURVE ( 'NONE', #2044, #11740, #18384, .T. ) ;
#12605 = ORIENTED_EDGE ( 'NONE', *, *, #1261, .T. ) ;
#12606 = VECTOR ( 'NONE', #12403, 1000.000000000000114 ) ;
#12607 = CARTESIAN_POINT ( 'NONE',  ( -90.00000000000000000, 0.000000000000000000, 0.000000000000000000 ) ) ;
#12608 = CARTESIAN_POINT ( 'NONE',  ( 3.458734125000000326, 1.432654583217640498, -2.699999998634404541 ) ) ;
#12609 = DIRECTION ( 'NONE',  ( -0.3373062947069096484, 0.9413949561959079615, 0.000000000000000000 ) ) ;
#12610 = VERTEX_POINT ( 'NONE', #8181 ) ;
#12611 = CARTESIAN_POINT ( 'NONE',  ( -35.00000000000000000, 4.500000000000001776, -19.99999999999998934 ) ) ;
#12612 = ORIENTED_EDGE ( 'NONE', *, *, #15979, .F. ) ;
#12613 = DIRECTION ( 'NONE',  ( 1.224646799147353207E-16, -0.000000000000000000, 1.000000000000000000 ) ) ;
#12614 = AXIS2_PLACEMENT_3D ( 'NONE', #7904, #13540, #7792 ) ;
#12615 = CARTESIAN_POINT ( 'NONE',  ( 4.000000000000000888, 4.898587196589412829E-16, 17.50000000000001066 ) ) ;
#12616 = CARTESIAN_POINT ( 'NONE',  ( 5.000000000000000888, 5.400000000000000355, 1.000000000000000000 ) ) ;
#12617 = DIRECTION ( 'NONE',  ( 0.000000000000000000, 0.000000000000000000, -1.000000000000000000 ) ) ;
#12618 = FACE_OUTER_BOUND ( 'NONE', #1627, .T. ) ;
#12619 = CIRCLE ( 'NONE', #17936, 4.000000000000002665 ) ;
#12620 = DIRECTION ( 'NONE',  ( 1.000000000000000000, 0.000000000000000000, 0.000000000000000000 ) ) ;
#12621 = AXIS2_PLACEMENT_3D ( 'NONE', #6588, #22984, #10321 ) ;
#12622 = CARTESIAN_POINT ( 'NONE',  ( -66.59999999999999432, 11.76776695296636888, 13.23223304703362579 ) ) ;
#12623 = EDGE_CURVE ( 'NONE', #21726, #15944, #15946, .T. ) ;
#12624 = CARTESIAN_POINT ( 'NONE',  ( 8.673617379884035472E-16, 4.618802153517012954, 0.000000000000000000 ) ) ;
#12625 = CARTESIAN_POINT ( 'NONE',  ( 60.00000000000004974, 12.13806810308082440, 17.37563432761511706 ) ) ;
#12626 = CARTESIAN_POINT ( 'NONE',  ( -3.458734124999999437, 0.000000000000000000, 19.68750000136560629 ) ) ;
#12627 = CARTESIAN_POINT ( 'NONE',  ( 60.00000000000000711, -15.00000000000000000, 10.00000000000007105 ) ) ;
#12628 = AXIS2_PLACEMENT_3D ( 'NONE', #12906, #16021, #21966 ) ;
#12629 = CARTESIAN_POINT ( 'NONE',  ( 4.000000000000000000, 4.898587196589412829E-16, 4.800000000000000711 ) ) ;
#12630 = CARTESIAN_POINT ( 'NONE',  ( -66.10000000109246798, 7.933012699999995476, 14.14382582708705094 ) ) ;
#12631 = CARTESIAN_POINT ( 'NONE',  ( 68.50000000218494733, 11.76776695296636888, 16.76776695296636532 ) ) ;
#12632 = CARTESIAN_POINT ( 'NONE',  ( -3.458734124999998993, 0.000000000000000000, 16.43750000136560629 ) ) ;
#12633 = FACE_OUTER_BOUND ( 'NONE', #12397, .T. ) ;
#12634 = EDGE_CURVE ( 'NONE', #8256, #5464, #23112, .T. ) ;
#12635 = EDGE_CURVE ( 'NONE', #10125, #1357, #1081, .T. ) ;
#12636 = VERTEX_POINT ( 'NONE', #19178 ) ;
#12637 = VERTEX_POINT ( 'NONE', #19058 ) ;
#12638 = CARTESIAN_POINT ( 'NONE',  ( 56.68518183416157541, 10.06805114094561659, 10.99999999999999645 ) ) ;
#12639 = CARTESIAN_POINT ( 'NONE',  ( -68.45000000109247651, 9.999999999999998224, 12.93301269999999192 ) ) ;
#12640 = CARTESIAN_POINT ( 'NONE',  ( 0.000000000000000000, 0.000000000000000000, 0.000000000000000000 ) ) ;
#12641 = AXIS2_PLACEMENT_3D ( 'NONE', #9714, #6106, #7686 ) ;
#12642 = CARTESIAN_POINT ( 'NONE',  ( -4.000000000000000000, 0.000000000000000000, -2.574999997268812457 ) ) ;
#12643 = ORIENTED_EDGE ( 'NONE', *, *, #22492, .F. ) ;
#12644 = CIRCLE ( 'NONE', #7662, 8.749000000000002331 ) ;
#12645 = VERTEX_POINT ( 'NONE', #6253 ) ;
#12646 = LINE ( 'NONE', #3728, #11383 ) ;
#12647 = CARTESIAN_POINT ( 'NONE',  ( 50.28356816583843880, 8.689308171935074654, 12.02818770551464489 ) ) ;
#12648 = CARTESIAN_POINT ( 'NONE',  ( -72.05000000109247082, 9.999999999999998224, 17.06698730000000097 ) ) ;
#12649 = CARTESIAN_POINT ( 'NONE',  ( -68.80000000109247082, 12.06698730000000275, 14.14382582708705094 ) ) ;
#12650 = CARTESIAN_POINT ( 'NONE',  ( -2.445694354108818303, -2.445694354108820967, 14.81250000136560452 ) ) ;
#12651 = CARTESIAN_POINT ( 'NONE',  ( 4.000000000000001776, -1.656854249492379694, 11.56250000273119838 ) ) ;
#12652 = CARTESIAN_POINT ( 'NONE',  ( 60.81018183416157541, 12.99999999999999822, 15.06805114094562192 ) ) ;
#12653 = DIRECTION ( 'NONE',  ( -1.000000000000000000, -0.000000000000000000, 0.000000000000000000 ) ) ;
#12654 = CIRCLE ( 'NONE', #20646, 2.041999999999999815 ) ;
#12655 = EDGE_CURVE ( 'NONE', #1035, #2408, #19524, .T. ) ;
#12656 = CARTESIAN_POINT ( 'NONE',  ( 53.06250000000000711, 6.999999999999997335, 15.00000000000000533 ) ) ;
#12657 = CARTESIAN_POINT ( 'NONE',  ( 6.353591512924457348E-16, -3.458734125000000770, -1.762499998634403209 ) ) ;
#12658 = CARTESIAN_POINT ( 'NONE',  ( -2.828427124746189403, 2.828427124746190291, 18.00000000273119483 ) ) ;
#12659 = EDGE_CURVE ( 'NONE', #4081, #18467, #22964, .T. ) ;
#12660 = DIRECTION ( 'NONE',  ( -1.000000000000000000, -0.000000000000000000, -0.000000000000000000 ) ) ;
#12661 = CIRCLE ( 'NONE', #20650, 2.649999999999999467 ) ;
#12662 = EDGE_CURVE ( 'NONE', #18572, #20917, #13929, .T. ) ;
#12663 = VERTEX_POINT ( 'NONE', #8295 ) ;
#12664 = PLANE ( 'NONE',  #20517 ) ;
#12665 = FACE_OUTER_BOUND ( 'NONE', #21596, .T. ) ;
#12666 = ORIENTED_EDGE ( 'NONE', *, *, #10543, .F. ) ;
#12667 = CARTESIAN_POINT ( 'NONE',  ( 55.12500000000000711, 12.12132034355964727, 17.12132034355963484 ) ) ;
#12669 = AXIS2_PLACEMENT_3D ( 'NONE', #20853, #4344, #12145 ) ;
#12668 = FILL_AREA_STYLE ('',( #1715 ) ) ;
#12670 = CARTESIAN_POINT ( 'NONE',  ( 3.458734125000000770, -1.432654583217639610, 5.175000001365595459 ) ) ;
#12671 = FACE_OUTER_BOUND ( 'NONE', #1026, .T. ) ;
#12672 = EDGE_LOOP ( 'NONE', ( #22367, #21008 ) ) ;
#12673 = CARTESIAN_POINT ( 'NONE',  ( -3.999999999999998224, -1.656854249492383246, 18.06250000000001421 ) ) ;
#12674 = VERTEX_POINT ( 'NONE', #9990 ) ;
#12675 = CARTESIAN_POINT ( 'NONE',  ( 4.999999999999999112, -7.958834565716711218, -7.593217523260670454 ) ) ;
#12676 = CARTESIAN_POINT ( 'NONE',  ( 4.000000000000000000, 4.898587196589412829E-16, -3.074999997268812901 ) ) ;
#12677 = VERTEX_POINT ( 'NONE', #17281 ) ;
#12678 = PLANE ( 'NONE',  #12993 ) ;
#12679 = DIRECTION ( 'NONE',  ( -1.000000000000000000, 0.000000000000000000, 0.000000000000000000 ) ) ;
#12680 = EDGE_LOOP ( 'NONE', ( #14128, #17409, #4815, #13624 ) ) ;
#12681 = CARTESIAN_POINT ( 'NONE',  ( 66.45000000109247651, 9.999999999999998224, 17.06698730000000097 ) ) ;
#12682 = VECTOR ( 'NONE', #10817, 1000.000000000000000 ) ;
#12683 = PRESENTATION_LAYER_ASSIGNMENT (  '', '', ( #6537 ) ) ;
#12684 = CARTESIAN_POINT ( 'NONE',  ( 70.39999999999999147, 8.232233047033629347, 13.23223304703362402 ) ) ;
#12685 = CYLINDRICAL_SURFACE ( 'NONE', #20783, 4.000000000000000000 ) ;
#12686 = CARTESIAN_POINT ( 'NONE',  ( 69.50000000218494733, 8.232233047033627571, 16.76776695296636532 ) ) ;
#12687 = EDGE_CURVE ( 'NONE', #5642, #5980, #11909, .T. ) ;
#12688 = CARTESIAN_POINT ( 'NONE',  ( 55.90856816583843880, 13.97181229448534978, 13.27509460956196641 ) ) ;
#12689 = CARTESIAN_POINT ( 'NONE',  ( 3.458734125000000770, -1.432654583217639610, -0.8249999986344030978 ) ) ;
#12690 = CARTESIAN_POINT ( 'NONE',  ( -3.458734124999998105, 1.432654583217640276, 12.37500000136560629 ) ) ;
#12691 = B_SPLINE_CURVE_WITH_KNOTS ( 'NONE', 3,
 ( #15540, #17441, #17556, #15656, #22928 ),
 .UNSPECIFIED., .F., .F.,
 ( 4, 1, 4 ),
 ( 5.640274452250024914E-20, 0.002309401076758505356, 0.004618802153517010713 ),
 .UNSPECIFIED. ) ;
#12692 = CARTESIAN_POINT ( 'NONE',  ( -3.999999999999998224, -1.656854249492383024, 18.18750000273119483 ) ) ;
#12693 = DIRECTION ( 'NONE',  ( 1.000000000000000000, -0.000000000000000000, -0.000000000000000000 ) ) ;
#12694 = ORIENTED_EDGE ( 'NONE', *, *, #19940, .T. ) ;
#12695 = PLANE ( 'NONE',  #13423 ) ;
#12696 = PLANE ( 'NONE',  #23167 ) ;
#12697 = CARTESIAN_POINT ( 'NONE',  ( 4.999999999999999112, -8.152713396088785203, 3.174628368996045946 ) ) ;
#12698 = CIRCLE ( 'NONE', #11554, 2.500000000000007550 ) ;
#12699 = EDGE_LOOP ( 'NONE', ( #6422, #2250, #5645, #23022 ) ) ;
#12700 = ORIENTED_EDGE ( 'NONE', *, *, #9661, .T. ) ;
#12701 = PLANE ( 'NONE',  #11404 ) ;
#12702 = CARTESIAN_POINT ( 'NONE',  ( 56.90625000000000711, 13.99999999999999289, 13.34314575050759544 ) ) ;
#12703 = VERTEX_POINT ( 'NONE', #10348 ) ;
#12704 = DIRECTION ( 'NONE',  ( 1.000000000000000000, 0.000000000000000000, 0.000000000000000000 ) ) ;
#12705 = ORIENTED_EDGE ( 'NONE', *, *, #247, .T. ) ;
#12706 = EDGE_CURVE ( 'NONE', #3785, #15043, #22216, .T. ) ;
#12707 = CARTESIAN_POINT ( 'NONE',  ( 51.46875000000000000, 5.999999999999987566, 13.34314575050763452 ) ) ;
#12708 = CARTESIAN_POINT ( 'NONE',  ( 66.60000000218495586, 9.999999999999998224, 12.49999999999999289 ) ) ;
#12709 = CYLINDRICAL_SURFACE ( 'NONE', #12256, 2.500000000000002220 ) ;
#12710 = CARTESIAN_POINT ( 'NONE',  ( 0.000000000000000000, 0.000000000000000000, 0.000000000000000000 ) ) ;
#12711 = DIRECTION ( 'NONE',  ( 1.000000000000000000, 0.000000000000000000, 0.000000000000000000 ) ) ;
#12712 = VERTEX_POINT ( 'NONE', #1786 ) ;
#12713 = CARTESIAN_POINT ( 'NONE',  ( 1.971781867644420635E-15, -4.000000000000000000, 17.37500000273119483 ) ) ;
#12714 = FACE_OUTER_BOUND ( 'NONE', #2523, .T. ) ;
#12715 = CARTESIAN_POINT ( 'NONE',  ( 60.99768183416157541, 12.87654654797631792, 12.21969229848393113 ) ) ;
#12716 = CARTESIAN_POINT ( 'NONE',  ( 2.149058192116893196, -6.264794173742287420, -3.633174458636617477 ) ) ;
#12717 = CARTESIAN_POINT ( 'NONE',  ( 66.10000000109246798, 7.933012699999995476, 14.14382582708705094 ) ) ;
#12718 = CARTESIAN_POINT ( 'NONE',  ( -67.79999999999999716, 8.232233047033627571, 16.76776695296636532 ) ) ;
#12719 = DIRECTION ( 'NONE',  ( -0.000000000000000000, -0.000000000000000000, 1.000000000000000000 ) ) ;
#12720 = ORIENTED_EDGE ( 'NONE', *, *, #4832, .T. ) ;
#12721 = CARTESIAN_POINT ( 'NONE',  ( -19.99999999999999645, -9.000000000000003553, 5.000000000000079936 ) ) ;
#12722 = CARTESIAN_POINT ( 'NONE',  ( 58.87500000000000711, 7.878679656440349177, 12.87867965644035984 ) ) ;
#12723 = CARTESIAN_POINT ( 'NONE',  ( -14.16125006966725053, -11.25000000000000355, 5.000000000000079936 ) ) ;
#12724 = CARTESIAN_POINT ( 'NONE',  ( -72.20000000000000284, 11.76776695296636888, 13.23223304703362579 ) ) ;
#12725 = ORIENTED_EDGE ( 'NONE', *, *, #455, .F. ) ;
#12726 = CARTESIAN_POINT ( 'NONE',  ( -65.00000000000000000, -10.00000000000000178, 14.99999999999999467 ) ) ;
#12727 = CARTESIAN_POINT ( 'NONE',  ( 43.27628836966725601, -11.25000000000000355, 5.000000000000079936 ) ) ;
#12728 = LINE ( 'NONE', #3583, #5157 ) ;
#12729 = ORIENTED_EDGE ( 'NONE', *, *, #8393, .T. ) ;
#12730 = CARTESIAN_POINT ( 'NONE',  ( 1.236993788156008760E-15, 0.000000000000000000, 21.31370849898476649 ) ) ;
#12731 = ORIENTED_EDGE ( 'NONE', *, *, #16288, .T. ) ;
#12732 = EDGE_CURVE ( 'NONE', #19018, #22332, #23341, .T. ) ;
#12733 = CARTESIAN_POINT ( 'NONE',  ( 4.000000000000000888, 4.898587196589412829E-16, 18.50000000000001066 ) ) ;
#12734 = CARTESIAN_POINT ( 'NONE',  ( -2.828427124746189403, 2.828427124746190291, 18.87500000000001066 ) ) ;
#12735 = CARTESIAN_POINT ( 'NONE',  ( -66.19999999999998863, 8.232233047033627571, 16.76776695296636532 ) ) ;
#12736 = CARTESIAN_POINT ( 'NONE',  ( -1.519999999999999796, 8.239200000000002078, 0.000000000000000000 ) ) ;
#12737 = FILL_AREA_STYLE_COLOUR ( '', #22872 ) ;
#12738 = EDGE_CURVE ( 'NONE', #10634, #438, #8087, .T. ) ;
#12739 = CARTESIAN_POINT ( 'NONE',  ( -60.00000000000000711, 9.999999999999998224, 20.00000000000001421 ) ) ;
#12740 = CARTESIAN_POINT ( 'NONE',  ( -66.09999999999999432, 9.999999999999998224, 17.49999999999999645 ) ) ;
#12741 = CARTESIAN_POINT ( 'NONE',  ( -2.828427124746189403, -2.828427124746190735, -0.4499999972688122352 ) ) ;
#12742 = CARTESIAN_POINT ( 'NONE',  ( -2.445694354108818303, -2.445694354108820523, 18.56250000136560629 ) ) ;
#12743 = DIRECTION ( 'NONE',  ( 7.087422195345011518E-32, 1.000000000000000000, -0.000000000000000000 ) ) ;
#12744 = CARTESIAN_POINT ( 'NONE',  ( 4.000000000000000000, 1.656854249492381248, 3.862500000000005151 ) ) ;
#12745 = CARTESIAN_POINT ( 'NONE',  ( 4.999999999999999112, 4.472189673936787457, 8.264486777890123648 ) ) ;
#12746 = CARTESIAN_POINT ( 'NONE',  ( 1.025207404391860050E-15, 3.458734125000000326, 19.18750000136560629 ) ) ;
#12747 = DIRECTION ( 'NONE',  ( -1.000000000000000000, 0.000000000000000000, -0.000000000000000000 ) ) ;
#12748 = ORIENTED_EDGE ( 'NONE', *, *, #17282, .F. ) ;
#12749 = CARTESIAN_POINT ( 'NONE',  ( -69.25000000109247367, 9.999999999999998224, 12.93301269999999192 ) ) ;
#12750 = ORIENTED_EDGE ( 'NONE', *, *, #12447, .F. ) ;
#12751 = CARTESIAN_POINT ( 'NONE',  ( 54.34143183416158251, 8.275094609562001935, 18.97181229448536044 ) ) ;
#12752 = CARTESIAN_POINT ( 'NONE',  ( -67.75000000109247367, 11.46158073645647235, 13.53841926354352232 ) ) ;
#12753 = CARTESIAN_POINT ( 'NONE',  ( 0.000000000000000000, 0.000000000000000000, 0.000000000000000000 ) ) ;
#12754 = LINE ( 'NONE', #10947, #10585 ) ;
#12755 = ORIENTED_EDGE ( 'NONE', *, *, #10128, .F. ) ;
#12756 = EDGE_CURVE ( 'NONE', #14629, #9317, #14164, .T. ) ;
#12757 = EDGE_CURVE ( 'NONE', #9212, #16229, #9130, .T. ) ;
#12758 = ORIENTED_EDGE ( 'NONE', *, *, #15576, .T. ) ;
#12759 = CARTESIAN_POINT ( 'NONE',  ( 53.93981816583844591, 10.06805114094563791, 17.99999999999999645 ) ) ;
#12760 = CARTESIAN_POINT ( 'NONE',  ( -69.60000000109249640, 10.85617417291294551, 17.06698729999999742 ) ) ;
#12761 = EDGE_CURVE ( 'NONE', #17390, #13999, #14401, .T. ) ;
#12762 = EDGE_CURVE ( 'NONE', #6076, #4468, #10795, .T. ) ;
#12763 = CARTESIAN_POINT ( 'NONE',  ( -69.75000000109245946, 11.46158073645647235, 16.46158073645647235 ) ) ;
#12764 = CARTESIAN_POINT ( 'NONE',  ( -3.458734124999999437, 0.000000000000000000, 12.68750000136560629 ) ) ;
#12765 = CARTESIAN_POINT ( 'NONE',  ( 2.828427124746192067, -2.828427124746189847, 10.50000000273119660 ) ) ;
#12766 = CARTESIAN_POINT ( 'NONE',  ( 60.43518183416157541, 9.931948859054372747, 17.99999999999999645 ) ) ;
#12767 = DIRECTION ( 'NONE',  ( -0.000000000000000000, -0.000000000000000000, 1.000000000000000000 ) ) ;
#12768 = CARTESIAN_POINT ( 'NONE',  ( 54.37500000000000711, 7.878679656440349177, 12.87867965644035984 ) ) ;
#12769 = DIRECTION ( 'NONE',  ( -1.000000000000000000, 0.000000000000000000, 0.000000000000000000 ) ) ;
#12770 = CARTESIAN_POINT ( 'NONE',  ( 2.500000000000000000, 2.357898499370431722, -2.818925648462311528E-15 ) ) ;
#12771 = AXIS2_PLACEMENT_3D ( 'NONE', #16056, #14268, #947 ) ;
#12772 = VERTEX_POINT ( 'NONE', #10927 ) ;
#12773 = DIRECTION ( 'NONE',  ( -7.087422195345011518E-32, -1.000000000000000000, -0.000000000000000000 ) ) ;
#12774 = CARTESIAN_POINT ( 'NONE',  ( 2.500000000000000000, 2.357898499370431722, -2.818925648462311528E-15 ) ) ;
#12775 = ORIENTED_EDGE ( 'NONE', *, *, #20736, .T. ) ;
#12776 = CARTESIAN_POINT ( 'NONE',  ( 54.28125000000000000, 8.757359312880703683, 11.99999999999999822 ) ) ;
#12777 = CARTESIAN_POINT ( 'NONE',  ( 2.828427124746190735, -2.828427124746189847, -2.199999997268812013 ) ) ;
#12778 = CIRCLE ( 'NONE', #13536, 8.073750000000021743 ) ;
#12779 = DIRECTION ( 'NONE',  ( -0.8660254037844382635, -0.5000000000000005551, 0.000000000000000000 ) ) ;
#12780 = ORIENTED_EDGE ( 'NONE', *, *, #21355, .F. ) ;
#12781 = CARTESIAN_POINT ( 'NONE',  ( 1.971781867644420635E-15, -4.000000000000000000, 18.25000000000001066 ) ) ;
#12782 = CARTESIAN_POINT ( 'NONE',  ( 2.435583919667260400, -11.25000000000000355, 5.000000000000079936 ) ) ;
#12783 = EDGE_CURVE ( 'NONE', #20740, #22551, #9013, .T. ) ;
#12784 = CYLINDRICAL_SURFACE ( 'NONE', #19413, 11.00000000000000000 ) ;
#12785 = ORIENTED_EDGE ( 'NONE', *, *, #12196, .T. ) ;
#12786 = DIRECTION ( 'NONE',  ( 0.000000000000000000, 0.000000000000000000, -1.000000000000000000 ) ) ;
#12787 = LINE ( 'NONE', #3535, #12558 ) ;
#12788 = CARTESIAN_POINT ( 'NONE',  ( 3.458734125000000770, 1.432654583217640498, 0.5500000013655963471 ) ) ;
#12789 = EDGE_CURVE ( 'NONE', #17390, #9624, #23475, .T. ) ;
#12790 = VECTOR ( 'NONE', #3767, 1000.000000000000000 ) ;
#12791 = CARTESIAN_POINT ( 'NONE',  ( 72.29999999999998295, 12.50000000000000000, 14.99999999999999645 ) ) ;
#12792 = VECTOR ( 'NONE', #9117, 1000.000000000000114 ) ;
#12793 = DIRECTION ( 'NONE',  ( -1.000000000000000000, 0.000000000000000000, 0.000000000000000000 ) ) ;
#12794 = CARTESIAN_POINT ( 'NONE',  ( 69.54999999999999716, 7.499999999999996447, 13.96446609406725514 ) ) ;
#12795 = CARTESIAN_POINT ( 'NONE',  ( 53.00231816583844591, 12.78030770151603868, 12.12345345202365188 ) ) ;
#12796 = CARTESIAN_POINT ( 'NONE',  ( -1.432654583217640942, -3.458734124999999882, 0.9250000013655964581 ) ) ;
#12797 = CARTESIAN_POINT ( 'NONE',  ( 45.00000000000000000, -10.00000000000001954, 17.50000000000002842 ) ) ;
#12798 = LINE ( 'NONE', #23431, #17042 ) ;
#12799 = CARTESIAN_POINT ( 'NONE',  ( 60.00000000000000711, 9.999999999999998224, 19.99999999999999645 ) ) ;
#12800 = ORIENTED_EDGE ( 'NONE', *, *, #20920, .T. ) ;
#12801 = PLANE ( 'NONE',  #21795 ) ;
#12802 = DIRECTION ( 'NONE',  ( 0.000000000000000000, 0.000000000000000000, -1.000000000000000000 ) ) ;
#12803 = ORIENTED_EDGE ( 'NONE', *, *, #15979, .T. ) ;
#12804 = ORIENTED_EDGE ( 'NONE', *, *, #5375, .F. ) ;
#12805 = DIRECTION ( 'NONE',  ( 1.000000000000000000, 0.000000000000000000, 0.000000000000000000 ) ) ;
#12806 = ORIENTED_EDGE ( 'NONE', *, *, #7596, .F. ) ;
#12807 = CARTESIAN_POINT ( 'NONE',  ( 54.09375000000000711, 11.65685424949236015, 10.99999999999998579 ) ) ;
#12808 = ORIENTED_EDGE ( 'NONE', *, *, #5722, .T. ) ;
#12809 = LINE ( 'NONE', #7298, #7243 ) ;
#12810 = ORIENTED_EDGE ( 'NONE', *, *, #11990, .T. ) ;
#12811 = CARTESIAN_POINT ( 'NONE',  ( 52.43981816583844591, 10.06805114094564857, 19.00000000000000000 ) ) ;
#12812 = EDGE_CURVE ( 'NONE', #10320, #19958, #11410, .T. ) ;
#12813 = CARTESIAN_POINT ( 'NONE',  ( 68.50000000218494733, 11.76776695296636888, 16.76776695296636532 ) ) ;
#12814 = LINE ( 'NONE', #11009, #22921 ) ;
#12815 =( BOUNDED_CURVE ( )  B_SPLINE_CURVE ( 2, ( #6536, #11822, #17986, #13611, #1119, #13964, #776, #12058, #8463 ),
 .UNSPECIFIED., .F., .F. ) 
 B_SPLINE_CURVE_WITH_KNOTS ( ( 3, 2, 2, 2, 3 ),
 ( 0.1249999999999992367, 0.1406249999999996947, 0.1562500000000001388, 0.1718750000000005829, 0.1875000000000010270 ),
 .UNSPECIFIED. ) 
 CURVE ( )  GEOMETRIC_REPRESENTATION_ITEM ( )  RATIONAL_B_SPLINE_CURVE ( ( 1.000000000000003775, 0.9238795325112830747, 1.000000000000000000, 0.9238795325112867385, 1.000000000000000000, 0.9238795325112867385, 1.000000000000000000, 0.9238795325112817425, 1.000000000000005107 ) ) 
 REPRESENTATION_ITEM ( '' )  );
#12816 = DIRECTION ( 'NONE',  ( -1.000000000000000000, -0.000000000000000000, 0.000000000000000000 ) ) ;
#12817 = CARTESIAN_POINT ( 'NONE',  ( -2.828427124746189403, -2.828427124746190735, -0.5749999999999974021 ) ) ;
#12818 = VERTEX_POINT ( 'NONE', #5508 ) ;
#12819 = CARTESIAN_POINT ( 'NONE',  ( 2.828427124746192067, -2.828427124746189847, 18.50000000273119483 ) ) ;
#12820 = DIRECTION ( 'NONE',  ( -1.000000000000000000, -7.703719777548943412E-32, 0.000000000000000000 ) ) ;
#12821 = CARTESIAN_POINT ( 'NONE',  ( 53.31018183416157541, 14.00000000000000000, 15.06805114094561304 ) ) ;
#12822 = CARTESIAN_POINT ( 'NONE',  ( 3.548171615569589044, -1.118847994424759351, 2.039999999999997371 ) ) ;
#12823 = DIRECTION ( 'NONE',  ( 1.000000000000000000, 0.000000000000000000, 0.000000000000000000 ) ) ;
#12824 = FACE_OUTER_BOUND ( 'NONE', #13717, .T. ) ;
#12825 = CARTESIAN_POINT ( 'NONE',  ( 6.499999999999999112, -3.752776749732574135, -3.119443416399232394 ) ) ;
#12826 = ORIENTED_EDGE ( 'NONE', *, *, #8960, .T. ) ;
#12827 = CARTESIAN_POINT ( 'NONE',  ( -0.7789945309248447192, 3.375565665863409670, -3.295601554149322432 ) ) ;
#12828 = CARTESIAN_POINT ( 'NONE',  ( 52.87500000000000711, 7.878679656440349177, 12.87867965644035984 ) ) ;
#12829 = CARTESIAN_POINT ( 'NONE',  ( 4.999999999999999112, -8.264486777890077462, -4.472189673936873611 ) ) ;
#12830 = EDGE_LOOP ( 'NONE', ( #8971, #11001, #9178, #11036 ) ) ;
#12831 = DIRECTION ( 'NONE',  ( 1.000000000000000000, 0.000000000000000000, 0.000000000000000000 ) ) ;
#12832 = CARTESIAN_POINT ( 'NONE',  ( -2.445694354108820523, 2.445694354108820523, -2.387499998634403653 ) ) ;
#12833 = CARTESIAN_POINT ( 'NONE',  ( 35.00000000000000000, 7.500000000000001776, -20.00000000000000355 ) ) ;
#12834 = AXIS2_PLACEMENT_3D ( 'NONE', #2450, #4621, #15777 ) ;
#12835 = VECTOR ( 'NONE', #17955, 1000.000000000000114 ) ;
#12836 = ORIENTED_EDGE ( 'NONE', *, *, #18852, .F. ) ;
#12837 = LINE ( 'NONE', #18434, #4931 ) ;
#12838 = EDGE_LOOP ( 'NONE', ( #15358, #5974, #20856, #14273, #20410, #13304 ) ) ;
#12839 = CARTESIAN_POINT ( 'NONE',  ( -1.656854249492381248, -3.999999999999999112, 1.487500000000001155 ) ) ;
#12840 = CARTESIAN_POINT ( 'NONE',  ( 2.828427124746191179, 2.828427124746190291, 16.62500000000001066 ) ) ;
#12841 = DIRECTION ( 'NONE',  ( -0.000000000000000000, 1.000000000000000000, -0.000000000000000000 ) ) ;
#12842 = CARTESIAN_POINT ( 'NONE',  ( -27.50000000000000711, 7.500000000000001776, -33.66025403784446723 ) ) ;
#12843 = FILL_AREA_STYLE ('',( #12737 ) ) ;
#12844 = ORIENTED_EDGE ( 'NONE', *, *, #9683, .F. ) ;
#12845 = CARTESIAN_POINT ( 'NONE',  ( -68.09999999999999432, 9.999999999999998224, 12.49999999999999289 ) ) ;
#12846 = AXIS2_PLACEMENT_3D ( 'NONE', #329, #13290, #677 ) ;
#12847 = CARTESIAN_POINT ( 'NONE',  ( 2.499999999999999556, -9.915734732513254102, 4.762163868918236176 ) ) ;
#12848 = CARTESIAN_POINT ( 'NONE',  ( 71.95000000109247651, 11.46158073645647235, 13.53841926354352232 ) ) ;
#12849 = CARTESIAN_POINT ( 'NONE',  ( 2.445694354108821855, -2.445694354108820079, 17.81250000136560274 ) ) ;
#12850 = CARTESIAN_POINT ( 'NONE',  ( 4.198928548860774157, -0.8158838809860124996, -3.526471437616918170 ) ) ;
#12851 = ADVANCED_FACE ( 'NONE', ( #5274 ), #3236, .T. ) ;
#12852 = CARTESIAN_POINT ( 'NONE',  ( -4.000000000000000888, 1.656854249492380804, 6.237500000000001599 ) ) ;
#12853 = DIRECTION ( 'NONE',  ( -7.087422195345011518E-32, -1.000000000000000000, -0.000000000000000000 ) ) ;
#12854 = CARTESIAN_POINT ( 'NONE',  ( 2.445694354108821411, 2.445694354108820523, 14.06250000136560452 ) ) ;
#12855 = DIRECTION ( 'NONE',  ( -1.000000000000000000, 0.000000000000000000, 0.000000000000000000 ) ) ;
#12856 = APPLICATION_CONTEXT ( 'automotive_design' ) ;
#12857 = EDGE_LOOP ( 'NONE', ( #16538, #4024, #3584, #23497 ) ) ;
#12858 = CARTESIAN_POINT ( 'NONE',  ( -68.50000000109247367, 10.85617417291294551, 12.93301269999999192 ) ) ;
#12859 = ORIENTED_EDGE ( 'NONE', *, *, #6828, .T. ) ;
#12860 = CARTESIAN_POINT ( 'NONE',  ( 57.34143183416159673, 8.275094609562001935, 18.97181229448536044 ) ) ;
#12861 = CARTESIAN_POINT ( 'NONE',  ( -70.00000000109247367, 7.933012699999995476, 15.85617417291294196 ) ) ;
#12862 = DIRECTION ( 'NONE',  ( 0.000000000000000000, 0.000000000000000000, 1.000000000000000000 ) ) ;
#12863 = EDGE_CURVE ( 'NONE', #9354, #12095, #17637, .T. ) ;
#12864 = LINE ( 'NONE', #7463, #8260 ) ;
#12865 = ORIENTED_EDGE ( 'NONE', *, *, #11151, .F. ) ;
#12866 = VECTOR ( 'NONE', #9653, 1000.000000000000114 ) ;
#12867 = VERTEX_POINT ( 'NONE', #12616 ) ;
#12868 = VECTOR ( 'NONE', #4402, 1000.000000000000000 ) ;
#12869 = DIRECTION ( 'NONE',  ( 1.000000000000000000, -0.000000000000000000, -0.000000000000000000 ) ) ;
#12870 = CARTESIAN_POINT ( 'NONE',  ( 51.22106816583844591, 13.02818770551464489, 16.17458954617363531 ) ) ;
#12871 = CARTESIAN_POINT ( 'NONE',  ( -71.65000000109247935, 9.999999999999998224, 12.93301269999999192 ) ) ;
#12872 = CARTESIAN_POINT ( 'NONE',  ( -70.75000000109247367, 8.538419263543522320, 16.46158073645647235 ) ) ;
#12873 = CARTESIAN_POINT ( 'NONE',  ( 1.872352939448454495E-15, -3.458734125000000770, 11.93750000136560629 ) ) ;
#12874 = DIRECTION ( 'NONE',  ( -1.000000000000000000, -7.703719777548943412E-32, 0.000000000000000000 ) ) ;
#12875 = CARTESIAN_POINT ( 'NONE',  ( 51.75000000000000711, 7.878679656440361612, 17.12132034355964549 ) ) ;
#12876 = LINE ( 'NONE', #14676, #9121 ) ;
#12877 = EDGE_CURVE ( 'NONE', #9313, #12663, #11040, .T. ) ;
#12878 = CARTESIAN_POINT ( 'NONE',  ( 54.00000000000000711, 12.12132034355963484, 12.87867965644034740 ) ) ;
#12879 = ADVANCED_FACE ( 'NONE', ( #21665 ), #1672, .T. ) ;
#12880 = CARTESIAN_POINT ( 'NONE',  ( 4.000000000000001776, -1.656854249492379694, 15.56250000273119660 ) ) ;
#12881 = DIRECTION ( 'NONE',  ( 0.000000000000000000, 0.000000000000000000, -1.000000000000000000 ) ) ;
#12882 = EDGE_LOOP ( 'NONE', ( #189, #20832, #18369, #11120, #19828 ) ) ;
#12883 = DIRECTION ( 'NONE',  ( 1.000000000000000000, 0.000000000000000000, 0.000000000000000000 ) ) ;
#12884 = CARTESIAN_POINT ( 'NONE',  ( -70.50000000000000000, 9.999999999999998224, 12.49999999999999289 ) ) ;
#12885 = ORIENTED_EDGE ( 'NONE', *, *, #455, .T. ) ;
#12886 = CARTESIAN_POINT ( 'NONE',  ( 52.12500000000000711, 12.12132034355964727, 17.12132034355963484 ) ) ;
#12887 = CARTESIAN_POINT ( 'NONE',  ( -1.656854249492381248, -3.999999999999999112, -2.387499997268812013 ) ) ;
#12888 = EDGE_CURVE ( 'NONE', #13665, #4526, #3589, .T. ) ;
#12889 = CARTESIAN_POINT ( 'NONE',  ( -5.969670414742689779, -4.058962678540106062, -0.4037800551813781058 ) ) ;
#12890 = ORIENTED_EDGE ( 'NONE', *, *, #11264, .F. ) ;
#12891 = CARTESIAN_POINT ( 'NONE',  ( 1.656854249492381470, 4.000000000000000000, 18.68750000000001066 ) ) ;
#12892 = DIRECTION ( 'NONE',  ( -1.000000000000000000, 0.000000000000000000, 0.000000000000000000 ) ) ;
#12893 = FACE_OUTER_BOUND ( 'NONE', #13100, .T. ) ;
#12894 = ORIENTED_EDGE ( 'NONE', *, *, #7773, .T. ) ;
#12895 = CARTESIAN_POINT ( 'NONE',  ( -18.12177574676618974, -9.000000000000003553, 5.000000000000079936 ) ) ;
#12896 = CARTESIAN_POINT ( 'NONE',  ( 1.236993788156008760E-15, 0.000000000000000000, 21.31370849898476649 ) ) ;
#12897 = CARTESIAN_POINT ( 'NONE',  ( -3.458734125000000326, -1.432654583217642497, 0.05000000136559583364 ) ) ;
#12898 = CARTESIAN_POINT ( 'NONE',  ( 67.54999999999999716, 12.50000000000000000, 16.03553390593273420 ) ) ;
#12899 = EDGE_CURVE ( 'NONE', #11306, #10762, #20100, .T. ) ;
#12900 = CARTESIAN_POINT ( 'NONE',  ( 4.999999999999999112, -6.772677083992425295, 5.538577986808878251 ) ) ;
#12901 = CARTESIAN_POINT ( 'NONE',  ( 4.999999999999999112, -8.734705317681630277, 0.4999240074894146790 ) ) ;
#12902 = CARTESIAN_POINT ( 'NONE',  ( 50.18981816583844591, 9.931948859054346102, 10.99999999999999467 ) ) ;
#12903 = ADVANCED_FACE ( 'NONE', ( #22372 ), #17009, .F. ) ;
#12904 = CARTESIAN_POINT ( 'NONE',  ( -2.117863837641485618E-16, 3.458734125000000326, -0.5124999986344038749 ) ) ;
#12905 = CARTESIAN_POINT ( 'NONE',  ( -3.458734124999999437, 1.432654583217640498, 16.62500000136560629 ) ) ;
#12906 = CARTESIAN_POINT ( 'NONE',  ( 0.000000000000000000, 4.472189673936787457, 8.264486777890123648 ) ) ;
#12907 = CARTESIAN_POINT ( 'NONE',  ( -1.800000000000000711, 7.592810154713614487E-16, 6.200000000000020606 ) ) ;
#12908 = DIRECTION ( 'NONE',  ( 7.087422195345011518E-32, 1.000000000000000000, 0.000000000000000000 ) ) ;
#12909 = EDGE_LOOP ( 'NONE', ( #21862, #20537 ) ) ;
#12910 = LINE ( 'NONE', #11232, #23327 ) ;
#12911 = DIRECTION ( 'NONE',  ( 0.000000000000000000, 0.000000000000000000, 1.000000000000000000 ) ) ;
#12912 = DIRECTION ( 'NONE',  ( -0.000000000000000000, -1.000000000000000000, -0.000000000000000000 ) ) ;
#12913 = EDGE_CURVE ( 'NONE', #4647, #2825, #16097, .T. ) ;
#12914 = ORIENTED_EDGE ( 'NONE', *, *, #2896, .T. ) ;
#12915 = EDGE_CURVE ( 'NONE', #7761, #1719, #17239, .T. ) ;
#12916 = ORIENTED_EDGE ( 'NONE', *, *, #19741, .F. ) ;
#12917 = B_SPLINE_CURVE_WITH_KNOTS ( 'NONE', 3,
 ( #5559, #13009, #18731, #16583, #16828, #2320, #12889, #3749 ),
 .UNSPECIFIED., .F., .F.,
 ( 4, 2, 2, 4 ),
 ( 0.003797433802554454115, 0.004743183970586247432, 0.005688934138618041182, 0.007580434474681629550 ),
 .UNSPECIFIED. ) ;
#12918 = CARTESIAN_POINT ( 'NONE',  ( 57.75000000000000000, 7.171572875253819923, 17.82842712474619873 ) ) ;
#12919 = VERTEX_POINT ( 'NONE', #2016 ) ;
#12920 = CARTESIAN_POINT ( 'NONE',  ( -20.00005080000000035, 7.347880794884120722E-16, 6.000000000000000888 ) ) ;
#12921 = VERTEX_POINT ( 'NONE', #22012 ) ;
#12922 = CONICAL_SURFACE ( 'NONE', #15971, 5.560781378645573980, 1.221730476396046816 ) ;
#12923 = VECTOR ( 'NONE', #21847, 1000.000000000000000 ) ;
#12924 = CARTESIAN_POINT ( 'NONE',  ( 51.59606816583843170, 11.58880310854672935, 10.97181229448534445 ) ) ;
#12925 = CARTESIAN_POINT ( 'NONE',  ( 70.95000000109247651, 11.46158073645647235, 13.53841926354352232 ) ) ;
#12926 = DIRECTION ( 'NONE',  ( -0.3420201433256622181, 0.9396926207859106484, 1.232595164407828100E-31 ) ) ;
#12927 = CARTESIAN_POINT ( 'NONE',  ( 72.10000000109246798, 12.06698730000000275, 15.85617417291294196 ) ) ;
#12928 = CARTESIAN_POINT ( 'NONE',  ( 45.00000000000000000, -15.00000000000001954, 11.00000000000008882 ) ) ;
#12929 = ORIENTED_EDGE ( 'NONE', *, *, #7030, .F. ) ;
#12930 = CARTESIAN_POINT ( 'NONE',  ( -1.656854249492380138, -3.999999999999999112, 16.31250000273119483 ) ) ;
#12931 = VECTOR ( 'NONE', #5870, 1000.000000000000000 ) ;
#12932 = FACE_OUTER_BOUND ( 'NONE', #18080, .T. ) ;
#12933 = CARTESIAN_POINT ( 'NONE',  ( 56.59143183416158962, 11.72490539043799984, 11.02818770551463246 ) ) ;
#12934 = CARTESIAN_POINT ( 'NONE',  ( -2.117863837641482907E-16, 3.458734125000000770, -3.284567702311016468 ) ) ;
#12935 = DIRECTION ( 'NONE',  ( 1.000000000000000000, 0.000000000000000000, 0.000000000000000000 ) ) ;
#12936 = MECHANICAL_DESIGN_GEOMETRIC_PRESENTATION_REPRESENTATION (  '', ( #4480 ), #2183 ) ;
#12937 = CARTESIAN_POINT ( 'NONE',  ( 39.91453229447491680, 12.80710635516961382, 10.00000000000008882 ) ) ;
#12938 = VECTOR ( 'NONE', #220, 1000.000000000000000 ) ;
#12939 = PLANE ( 'NONE',  #6945 ) ;
#12940 = EDGE_LOOP ( 'NONE', ( #5386, #14159, #7169, #16553 ) ) ;
#12941 = FACE_OUTER_BOUND ( 'NONE', #15803, .T. ) ;
#12942 = CARTESIAN_POINT ( 'NONE',  ( 52.21875000000001421, 13.00000000000000533, 16.24264068711927322 ) ) ;
#12943 = CARTESIAN_POINT ( 'NONE',  ( 0.2500000000000002220, 0.000000000000000000, 0.000000000000000000 ) ) ;
#12944 = SURFACE_STYLE_USAGE ( .BOTH. , #2125 ) ;
#12945 = EDGE_CURVE ( 'NONE', #9531, #16003, #14588, .T. ) ;
#12946 = EDGE_CURVE ( 'NONE', #11906, #438, #1356, .T. ) ;
#12947 = ORIENTED_EDGE ( 'NONE', *, *, #19782, .F. ) ;
#12948 = CARTESIAN_POINT ( 'NONE',  ( 0.000000000000000000, 0.000000000000000000, 19.04999999999996874 ) ) ;
#12949 = DIRECTION ( 'NONE',  ( 0.000000000000000000, 0.000000000000000000, -1.000000000000000000 ) ) ;
#12950 = CARTESIAN_POINT ( 'NONE',  ( -4.000000000000000000, 4.898587196589412829E-16, 19.04999999999996874 ) ) ;
#12951 = CARTESIAN_POINT ( 'NONE',  ( -6.989194030332740226, -11.25000000000000355, 5.000000000000079936 ) ) ;
#12952 = ORIENTED_EDGE ( 'NONE', *, *, #17805, .T. ) ;
#12953 = CARTESIAN_POINT ( 'NONE',  ( 4.000000000000000000, -2.309401076758514915, -3.433295621305383349 ) ) ;
#12954 = EDGE_LOOP ( 'NONE', ( #19274, #17787, #5713, #18344, #4563, #17188, #3352, #11148, #9216, #13408, #2517, #23075, #3406, #3906, #724, #8801 ) ) ;
#12955 = AXIS2_PLACEMENT_3D ( 'NONE', #13790, #9959, #21046 ) ;
#12956 =( BOUNDED_CURVE ( )  B_SPLINE_CURVE ( 2, ( #15130, #5641, #22391, #11182, #18456, #9375, #16665, #14893, #20474 ),
 .UNSPECIFIED., .F., .F. ) 
 B_SPLINE_CURVE_WITH_KNOTS ( ( 3, 2, 2, 2, 3 ),
 ( 0.6875000000000001110, 0.7031250000000000000, 0.7187500000000000000, 0.7343749999999998890, 0.7499999999999997780 ),
 .UNSPECIFIED. ) 
 CURVE ( )  GEOMETRIC_REPRESENTATION_ITEM ( )  RATIONAL_B_SPLINE_CURVE ( ( 0.9999999999999994449, 0.9238795325112872936, 1.000000000000000000, 0.9238795325112867385, 1.000000000000000000, 0.9238795325112867385, 1.000000000000000000, 0.9238795325112878487, 0.9999999999999988898 ) ) 
 REPRESENTATION_ITEM ( '' )  );
#12957 = CARTESIAN_POINT ( 'NONE',  ( 2.828427124746192067, -2.828427124746189847, 14.37500000000001066 ) ) ;
#12958 = CYLINDRICAL_SURFACE ( 'NONE', #20669, 4.000000000000000000 ) ;
#12959 = VECTOR ( 'NONE', #19084, 1000.000000000000000 ) ;
#12960 = VECTOR ( 'NONE', #17186, 1000.000000000000000 ) ;
#12961 = DIRECTION ( 'NONE',  ( 0.3420201433256622181, -0.9396926207859107594, 0.000000000000000000 ) ) ;
#12962 = MECHANICAL_DESIGN_GEOMETRIC_PRESENTATION_REPRESENTATION (  '', ( #14103 ), #18281 ) ;
#12963 = DIRECTION ( 'NONE',  ( 1.000000000000000000, 0.000000000000000000, 0.000000000000000000 ) ) ;
#12964 = SURFACE_STYLE_FILL_AREA ( #12843 ) ;
#12965 = VERTEX_POINT ( 'NONE', #109 ) ;
#12966 = CARTESIAN_POINT ( 'NONE',  ( -67.20000000000000284, 8.232233047033629347, 13.23223304703362402 ) ) ;
#12967 = LINE ( 'NONE', #1916, #9924 ) ;
#12968 = CARTESIAN_POINT ( 'NONE',  ( 67.90000000109246514, 12.06698730000000275, 15.85617417291294196 ) ) ;
#12969 = CARTESIAN_POINT ( 'NONE',  ( 3.458734125000001214, 1.432654583217640498, 18.00000000136560274 ) ) ;
#12970 = DIRECTION ( 'NONE',  ( -1.000000000000000000, -0.000000000000000000, -0.000000000000000000 ) ) ;
#12971 = AXIS2_PLACEMENT_3D ( 'NONE', #21668, #8894, #16188 ) ;
#12972 = CARTESIAN_POINT ( 'NONE',  ( 1.432654583217640276, 3.458734125000000770, -2.324999998634404097 ) ) ;
#12973 = DIRECTION ( 'NONE',  ( -1.000000000000000000, -0.000000000000000000, -0.000000000000000000 ) ) ;
#12974 = CARTESIAN_POINT ( 'NONE',  ( -3.458734124999998993, -1.432654583217642497, 13.50000000136560452 ) ) ;
#12975 = CARTESIAN_POINT ( 'NONE',  ( 50.38765154071656838, -8.974600000000002353, 10.00000000000008882 ) ) ;
#12976 = EDGE_LOOP ( 'NONE', ( #20354, #14773 ) ) ;
#12977 = AXIS2_PLACEMENT_3D ( 'NONE', #15343, #17475, #6337 ) ;
#12978 = CARTESIAN_POINT ( 'NONE',  ( -70.10000000109248219, 10.85617417291294551, 12.93301269999999192 ) ) ;
#12979 = ORIENTED_EDGE ( 'NONE', *, *, #11253, .T. ) ;
#12980 = CARTESIAN_POINT ( 'NONE',  ( 57.06018183416157541, 5.999999999999996447, 14.93194885905437808 ) ) ;
#12981 = CARTESIAN_POINT ( 'NONE',  ( -69.80000000109247082, 10.85617417291294551, 17.06698729999999742 ) ) ;
#12982 = APPLICATION_PROTOCOL_DEFINITION ( 'draft international standard', 'automotive_design', 1998, #3030 ) ;
#12983 = CIRCLE ( 'NONE', #11464, 11.00000000000000000 ) ;
#12984 = DIRECTION ( 'NONE',  ( -0.000000000000000000, -0.000000000000000000, -1.000000000000000000 ) ) ;
#12985 = ORIENTED_EDGE ( 'NONE', *, *, #8449, .F. ) ;
#12986 = ORIENTED_EDGE ( 'NONE', *, *, #7465, .T. ) ;
#12987 = CARTESIAN_POINT ( 'NONE',  ( 1.432654583217643163, -3.458734124999999882, 19.00000000136560629 ) ) ;
#12988 = CARTESIAN_POINT ( 'NONE',  ( 54.28125000000000000, 8.757359312880703683, 11.99999999999999822 ) ) ;
#12989 = CIRCLE ( 'NONE', #17940, 9.000000000000000000 ) ;
#12990 = EDGE_CURVE ( 'NONE', #21998, #872, #5377, .T. ) ;
#12991 = CARTESIAN_POINT ( 'NONE',  ( -71.95000000109247651, 11.46158073645647235, 16.46158073645647235 ) ) ;
#12992 = CARTESIAN_POINT ( 'NONE',  ( -70.10000000109245377, 7.933012699999995476, 14.14382582708705094 ) ) ;
#12993 = AXIS2_PLACEMENT_3D ( 'NONE', #7269, #14585, #10979 ) ;
#12994 = CARTESIAN_POINT ( 'NONE',  ( -3.458734124999999437, 0.000000000000000000, 11.68750000136560629 ) ) ;
#12995 = PLANE ( 'NONE',  #12272 ) ;
#12996 = CARTESIAN_POINT ( 'NONE',  ( 51.00000000000000711, 12.12132034355963484, 12.87867965644034740 ) ) ;
#12997 = CARTESIAN_POINT ( 'NONE',  ( 52.68750000000000711, 9.999999999999989342, 11.99999999999999467 ) ) ;
#12998 = CARTESIAN_POINT ( 'NONE',  ( -3.999999999999999112, 0.000000000000000000, 15.12500000273119660 ) ) ;
#12999 = AXIS2_PLACEMENT_3D ( 'NONE', #16535, #111, #21545 ) ;
#13000 = CARTESIAN_POINT ( 'NONE',  ( 68.84999999999998010, 8.964466094067214286, 12.50000000000004086 ) ) ;
#13001 = VECTOR ( 'NONE', #22232, 1000.000000000000000 ) ;
#13002 = ORIENTED_EDGE ( 'NONE', *, *, #20443, .T. ) ;
#13003 = CARTESIAN_POINT ( 'NONE',  ( 70.25000000000000000, 7.499999999999996447, 16.03553390593273775 ) ) ;
#13004 = CARTESIAN_POINT ( 'NONE',  ( -71.65000000218496723, 12.50000000000000000, 16.03553390593273775 ) ) ;
#13005 = ORIENTED_EDGE ( 'NONE', *, *, #13379, .T. ) ;
#13006 = CARTESIAN_POINT ( 'NONE',  ( 51.37500000000000711, 7.878679656440349177, 12.87867965644035984 ) ) ;
#13007 = SURFACE_SIDE_STYLE ('',( #9651 ) ) ;
#13008 = CARTESIAN_POINT ( 'NONE',  ( -2.449293598294706907E-16, 4.000000000000000000, -1.824999997268811791 ) ) ;
#13009 = CARTESIAN_POINT ( 'NONE',  ( -3.525817189091417170, -5.469921996229802907, 4.020583056300408003E-16 ) ) ;
#13010 = ORIENTED_EDGE ( 'NONE', *, *, #21331, .F. ) ;
#13011 = AXIS2_PLACEMENT_3D ( 'NONE', #21562, #5528, #12391 ) ;
#13012 = CARTESIAN_POINT ( 'NONE',  ( 4.000000000000000888, 4.898587196589412829E-16, 18.50000000000001066 ) ) ;
#13013 =( GEOMETRIC_REPRESENTATION_CONTEXT ( 3 ) GLOBAL_UNCERTAINTY_ASSIGNED_CONTEXT ( ( #23172 ) ) GLOBAL_UNIT_ASSIGNED_CONTEXT ( ( #4493, #1128, #6662 ) ) REPRESENTATION_CONTEXT ( 'NONE', 'WORKASPACE' ) );
#13014 = CARTESIAN_POINT ( 'NONE',  ( -2.117863837641485618E-16, 3.458734125000000770, -3.262499998634402765 ) ) ;
#13015 = VECTOR ( 'NONE', #1122, 1000.000000000000000 ) ;
#13016 = LINE ( 'NONE', #7498, #18676 ) ;
#13017 = ORIENTED_EDGE ( 'NONE', *, *, #3399, .T. ) ;
#13018 = ADVANCED_FACE ( 'NONE', ( #7909 ), #13080, .F. ) ;
#13019 = CARTESIAN_POINT ( 'NONE',  ( -19.99999999999999645, -9.000000000000003553, 10.00000000000008882 ) ) ;
#13020 = EDGE_CURVE ( 'NONE', #10715, #13567, #15226, .T. ) ;
#13021 = CIRCLE ( 'NONE', #3808, 2.500000000000002220 ) ;
#13022 = CARTESIAN_POINT ( 'NONE',  ( -2.445694354108820523, 2.445694354108820523, -0.1374999986344035974 ) ) ;
#13023 = CIRCLE ( 'NONE', #3441, 8.749000000000002331 ) ;
#13024 = CARTESIAN_POINT ( 'NONE',  ( 67.39999999999999147, 11.76776695296636888, 13.23223304703362579 ) ) ;
#13025 = ADVANCED_FACE ( 'NONE', ( #9713 ), #18800, .F. ) ;
#13026 = DIRECTION ( 'NONE',  ( -0.5000000000000016653, 0.8660254037844378194, 0.000000000000000000 ) ) ;
#13027 = CARTESIAN_POINT ( 'NONE',  ( -19.99999999999999645, -9.000000000000003553, 10.00000000000008882 ) ) ;
#13028 = CARTESIAN_POINT ( 'NONE',  ( 53.84606816583843880, 8.411196891453267099, 19.02818770551464667 ) ) ;
#13029 = CARTESIAN_POINT ( 'NONE',  ( -1.432654583217640942, -3.458734124999999882, 1.925000001365597457 ) ) ;
#13030 = CARTESIAN_POINT ( 'NONE',  ( 2.445694354108821411, 2.445694354108820523, 14.31250000136560452 ) ) ;
#13031 = CARTESIAN_POINT ( 'NONE',  ( 2.499999999999999556, 10.90201369670498721, 1.464956435139581403 ) ) ;
#13032 = CARTESIAN_POINT ( 'NONE',  ( -71.50000000109247367, 9.143825827087049163, 17.06698730000000097 ) ) ;
#13033 = FACE_OUTER_BOUND ( 'NONE', #18114, .T. ) ;
#13034 = EDGE_LOOP ( 'NONE', ( #20292, #15632, #960, #5615 ) ) ;
#13035 = CARTESIAN_POINT ( 'NONE',  ( 6.500000000000000888, -2.517290933526018737, -3.443420074781601059 ) ) ;
#13036 = DIRECTION ( 'NONE',  ( 0.9396926207859107594, -0.3420201433256623291, 3.697785493223492838E-32 ) ) ;
#13037 = PLANE ( 'NONE',  #13596 ) ;
#13038 = ORIENTED_EDGE ( 'NONE', *, *, #9394, .F. ) ;
#13039 = ORIENTED_EDGE ( 'NONE', *, *, #17410, .F. ) ;
#13040 = FACE_OUTER_BOUND ( 'NONE', #4825, .T. ) ;
#13041 = ADVANCED_FACE ( 'NONE', ( #584 ), #12958, .F. ) ;
#13042 = CARTESIAN_POINT ( 'NONE',  ( 55.12500000000000711, 12.82842712474620228, 17.82842712474617386 ) ) ;
#13043 = ORIENTED_EDGE ( 'NONE', *, *, #753, .F. ) ;
#13044 = DIRECTION ( 'NONE',  ( 0.3420201433256622181, -0.9396926207859107594, 0.000000000000000000 ) ) ;
#13045 = ORIENTED_EDGE ( 'NONE', *, *, #13752, .F. ) ;
#13046 = VECTOR ( 'NONE', #23596, 1000.000000000000000 ) ;
#13047 = CARTESIAN_POINT ( 'NONE',  ( 54.31481816583844591, 14.00000000000000178, 14.93194885905434610 ) ) ;
#13048 = EDGE_CURVE ( 'NONE', #5354, #1712, #22179, .T. ) ;
#13049 = STYLED_ITEM ( 'NONE', ( #13180 ), #19874 ) ;
#13050 = ADVANCED_FACE ( 'NONE', ( #2264 ), #2383, .T. ) ;
#13051 = CARTESIAN_POINT ( 'NONE',  ( 71.05000000109247082, 12.06698730000000097, 14.99999999999999645 ) ) ;
#13052 = CARTESIAN_POINT ( 'NONE',  ( 66.44999999999998863, 8.964466094067219615, 12.50000000000003553 ) ) ;
#13053 = CARTESIAN_POINT ( 'NONE',  ( 70.55000000109245661, 11.46158073645647235, 16.46158073645647235 ) ) ;
#13054 = EDGE_CURVE ( 'NONE', #10661, #14897, #4611, .T. ) ;
#13055 = ORIENTED_EDGE ( 'NONE', *, *, #7745, .T. ) ;
#13056 = CARTESIAN_POINT ( 'NONE',  ( -3.999999999999998224, -1.656854249492383246, 11.06250000000001066 ) ) ;
#13057 = EDGE_CURVE ( 'NONE', #19193, #14005, #7690, .T. ) ;
#13058 = CARTESIAN_POINT ( 'NONE',  ( 1.656854249492380138, 4.000000000000000000, 0.1125000027311862244 ) ) ;
#13059 = CARTESIAN_POINT ( 'NONE',  ( 56.02893183416158962, 11.58880310854676132, 19.02818770551463956 ) ) ;
#13060 = CARTESIAN_POINT ( 'NONE',  ( 3.736776272708129287, -0.5369652245313190075, 2.039999999999999147 ) ) ;
#13061 = CARTESIAN_POINT ( 'NONE',  ( 70.20000000218495018, 9.999999999999998224, 17.49999999999999645 ) ) ;
#13062 = DIRECTION ( 'NONE',  ( -1.000000000000000000, 0.000000000000000000, 1.224646799147353207E-16 ) ) ;
#13063 = CARTESIAN_POINT ( 'NONE',  ( -65.95000000109246230, 8.538419263543522320, 16.46158073645647235 ) ) ;
#13064 = CARTESIAN_POINT ( 'NONE',  ( -2.697128823393878161, 5.948365447239581272, -0.01372220897661629788 ) ) ;
#13065 = ORIENTED_EDGE ( 'NONE', *, *, #5867, .F. ) ;
#13066 = CARTESIAN_POINT ( 'NONE',  ( 0.000000000000000000, 5.538577986808900455, 6.772677083992405755 ) ) ;
#13067 = CARTESIAN_POINT ( 'NONE',  ( 53.62500000000000711, 12.12132034355964727, 17.12132034355963484 ) ) ;
#13068 = CYLINDRICAL_SURFACE ( 'NONE', #5443, 2.500000000000002220 ) ;
#13069 = ORIENTED_EDGE ( 'NONE', *, *, #15414, .T. ) ;
#13070 = DIRECTION ( 'NONE',  ( -1.000000000000000000, 0.000000000000000000, -0.000000000000000000 ) ) ;
#13071 = DIRECTION ( 'NONE',  ( -1.000000000000000000, -0.000000000000000000, -0.000000000000000000 ) ) ;
#13072 = CARTESIAN_POINT ( 'NONE',  ( 1.312671235360372224, 3.860931062424219462, -0.05923475698270440348 ) ) ;
#13073 = CARTESIAN_POINT ( 'NONE',  ( 4.000000000000000888, 4.898587196589412829E-16, 16.62500000273119838 ) ) ;
#13074 = ORIENTED_EDGE ( 'NONE', *, *, #3401, .T. ) ;
#13075 = CARTESIAN_POINT ( 'NONE',  ( 0.000000000000000000, -7.593217523260641144, 7.958834565716742304 ) ) ;
#13076 = ORIENTED_EDGE ( 'NONE', *, *, #5896, .F. ) ;
#13077 = CARTESIAN_POINT ( 'NONE',  ( 118.3095189484530181, 10.00000000000001599, 15.00000000000003020 ) ) ;
#13078 = EDGE_CURVE ( 'NONE', #2784, #16998, #472, .T. ) ;
#13079 = CARTESIAN_POINT ( 'NONE',  ( -3.999999999999999112, 0.000000000000000000, 14.00000000000001066 ) ) ;
#13080 = PLANE ( 'NONE',  #20266 ) ;
#13081 = CIRCLE ( 'NONE', #13798, 6.200000000000020606 ) ;
#13082 = PLANE ( 'NONE',  #4190 ) ;
#13083 = EDGE_CURVE ( 'NONE', #16416, #16674, #10764, .T. ) ;
#13084 = SURFACE_STYLE_FILL_AREA ( #22257 ) ;
#13085 = CARTESIAN_POINT ( 'NONE',  ( 69.60000000109246798, 12.06698729999999919, 14.14382582708705094 ) ) ;
#13086 = ORIENTED_EDGE ( 'NONE', *, *, #1544, .F. ) ;
#13087 = EDGE_CURVE ( 'NONE', #5522, #20911, #2846, .T. ) ;
#13088 = DIRECTION ( 'NONE',  ( 0.000000000000000000, 5.754033390038004481E-16, -1.000000000000000000 ) ) ;
#13089 = CARTESIAN_POINT ( 'NONE',  ( -20.00000000000001066, 4.500000000000003553, -50.00000000000000000 ) ) ;
#13090 = CARTESIAN_POINT ( 'NONE',  ( 65.90000000109246514, 7.933012699999995476, 14.14382582708705094 ) ) ;
#13091 = CARTESIAN_POINT ( 'NONE',  ( -2.445694354108818303, -2.445694354108820523, 15.56250000136560629 ) ) ;
#13092 = FACE_OUTER_BOUND ( 'NONE', #13565, .T. ) ;
#13093 = B_SPLINE_CURVE_WITH_KNOTS ( 'NONE', 3,
 ( #17126, #7798, #15115, #11878, #4893, #19607 ),
 .UNSPECIFIED., .F., .F.,
 ( 4, 2, 4 ),
 ( 0.01049192114530184475, 0.01239128608052813933, 0.01429065101575443392 ),
 .UNSPECIFIED. ) ;
#13094 = CARTESIAN_POINT ( 'NONE',  ( 3.458734125000001214, -1.432654583217639610, -1.574999998634403875 ) ) ;
#13095 = CARTESIAN_POINT ( 'NONE',  ( -4.000000000000000000, -1.656854249492383246, 4.362500000000001599 ) ) ;
#13096 = CARTESIAN_POINT ( 'NONE',  ( -1.432654583217639610, -3.458734124999999882, 11.62500000136560452 ) ) ;
#13097 = CARTESIAN_POINT ( 'NONE',  ( -7.000000000000000000, 8.572527594031473190E-16, 1.734723475976807094E-15 ) ) ;
#13098 = ORIENTED_EDGE ( 'NONE', *, *, #5499, .F. ) ;
#13099 = CARTESIAN_POINT ( 'NONE',  ( -68.55000000109247082, 11.46158073645647235, 13.53841926354352232 ) ) ;
#13100 = EDGE_LOOP ( 'NONE', ( #23536, #22008, #20094, #20414 ) ) ;
#13101 = CARTESIAN_POINT ( 'NONE',  ( 57.46875000000000711, 5.999999999999987566, 13.34314575050763452 ) ) ;
#13102 = CARTESIAN_POINT ( 'NONE',  ( -69.45000000109247651, 9.999999999999998224, 12.93301269999999192 ) ) ;
#13103 = ITEM_DEFINED_TRANSFORMATION ( 'NONE', 'NONE', #22146,  #7318 ) ;
#13104 =( BOUNDED_CURVE ( )  B_SPLINE_CURVE ( 2, ( #8119, #5942, #22328, #20883, #10153, #16964, #429, #15546, #893 ),
 .UNSPECIFIED., .F., .F. ) 
 B_SPLINE_CURVE_WITH_KNOTS ( ( 3, 2, 2, 2, 3 ),
 ( 0.5500000000000000444, 0.5625000000000000000, 0.5749999999999999556, 0.5875000000000000222, 0.5999999999999999778 ),
 .UNSPECIFIED. ) 
 CURVE ( )  GEOMETRIC_REPRESENTATION_ITEM ( )  RATIONAL_B_SPLINE_CURVE ( ( 1.000000000000000000, 0.9238795325112867385, 1.000000000000000000, 0.9238795325112867385, 1.000000000000000000, 0.9238795325112867385, 1.000000000000000000, 0.9238795325112867385, 1.000000000000000000 ) ) 
 REPRESENTATION_ITEM ( '' )  );
#13105 = ORIENTED_EDGE ( 'NONE', *, *, #4392, .T. ) ;
#13106 = VERTEX_POINT ( 'NONE', #20813 ) ;
#13107 = ORIENTED_EDGE ( 'NONE', *, *, #5991, .F. ) ;
#13108 = CARTESIAN_POINT ( 'NONE',  ( -3.458734124999998993, -1.432654583217642497, 15.75000000136560629 ) ) ;
#13109 = CARTESIAN_POINT ( 'NONE',  ( 53.71875000000002132, 13.00000000000000711, 16.24264068711927322 ) ) ;
#13110 = CARTESIAN_POINT ( 'NONE',  ( -70.20000000109246230, 12.06698730000000275, 14.14382582708705094 ) ) ;
#13111 = CARTESIAN_POINT ( 'NONE',  ( 70.10000000109248219, 10.85617417291294551, 12.93301269999999192 ) ) ;
#13112 = EDGE_CURVE ( 'NONE', #5198, #10249, #19146, .T. ) ;
#13113 = CARTESIAN_POINT ( 'NONE',  ( -69.60000000109248219, 12.06698730000000275, 14.14382582708705094 ) ) ;
#13114 = CARTESIAN_POINT ( 'NONE',  ( -1.432654583217639166, 3.458734125000000770, 10.50000000136560629 ) ) ;
#13115 = CARTESIAN_POINT ( 'NONE',  ( 4.999999999999999112, -6.807171995660539210, -6.478011392632959442 ) ) ;
#13116 = CARTESIAN_POINT ( 'NONE',  ( 54.00000000000000711, 12.12132034355963484, 12.87867965644034740 ) ) ;
#13117 = CARTESIAN_POINT ( 'NONE',  ( 72.00000000000000000, 8.232233047033629347, 13.23223304703362402 ) ) ;
#13118 = CARTESIAN_POINT ( 'NONE',  ( 54.56250000000000711, 6.999999999999997335, 15.00000000000000533 ) ) ;
#13119 = CARTESIAN_POINT ( 'NONE',  ( 49.55947366966726264, -11.25000000000000355, 10.00000000000008882 ) ) ;
#13120 = CARTESIAN_POINT ( 'NONE',  ( 1.656854249492384135, -3.999999999999999112, 16.43750000273119838 ) ) ;
#13121 = CARTESIAN_POINT ( 'NONE',  ( 33.85151041966726382, -11.25000000000000355, 5.000000000000079936 ) ) ;
#13122 = VERTEX_POINT ( 'NONE', #11756 ) ;
#13123 = CARTESIAN_POINT ( 'NONE',  ( 70.09999999999999432, 9.999999999999998224, 17.49999999999999645 ) ) ;
#13124 = CARTESIAN_POINT ( 'NONE',  ( -70.25000000000000000, 7.499999999999996447, 16.03553390593273775 ) ) ;
#13125 = ORIENTED_EDGE ( 'NONE', *, *, #14346, .F. ) ;
#13126 = CARTESIAN_POINT ( 'NONE',  ( 54.75000000000000711, 7.878679656440361612, 17.12132034355964549 ) ) ;
#13127 = CARTESIAN_POINT ( 'NONE',  ( -1.432654583217640942, -3.458734124999999882, 4.925000001365594571 ) ) ;
#13128 = VECTOR ( 'NONE', #20564, 1000.000000000000000 ) ;
#13129 = DIRECTION ( 'NONE',  ( 0.000000000000000000, 0.000000000000000000, 1.000000000000000000 ) ) ;
#13130 = VERTEX_POINT ( 'NONE', #14010 ) ;
#13131 = CARTESIAN_POINT ( 'NONE',  ( 2.828427124746192067, -2.828427124746189847, 12.37500000000001066 ) ) ;
#13132 = DIRECTION ( 'NONE',  ( -0.000000000000000000, -1.000000000000000000, -0.000000000000000000 ) ) ;
#13133 = LINE ( 'NONE', #20864, #18277 ) ;
#13134 = ORIENTED_EDGE ( 'NONE', *, *, #3794, .F. ) ;
#13135 = DIRECTION ( 'NONE',  ( -4.930380657631312836E-32, -0.3420201433256691015, -0.9396926207859083169 ) ) ;
#13136 = CARTESIAN_POINT ( 'NONE',  ( 3.458734125000000770, 1.432654583217640498, 1.550000001365597013 ) ) ;
#13137 = CARTESIAN_POINT ( 'NONE',  ( 69.59999999999999432, 8.232233047033629347, 13.23223304703362402 ) ) ;
#13138 = DIRECTION ( 'NONE',  ( 0.000000000000000000, 0.000000000000000000, -1.000000000000000000 ) ) ;
#13139 = CARTESIAN_POINT ( 'NONE',  ( -0.3208286057739654917, 4.433571671609680465, -0.3503314178412548774 ) ) ;
#13140 = CARTESIAN_POINT ( 'NONE',  ( 58.53356816583845301, 11.31069182806492712, 17.97181229448534623 ) ) ;
#13141 = CARTESIAN_POINT ( 'NONE',  ( -3.458734124999999882, -1.432654583217642497, -3.199999998634404985 ) ) ;
#13142 = CARTESIAN_POINT ( 'NONE',  ( 3.458734125000001658, 1.432654583217640498, 14.25000000136560629 ) ) ;
#13143 = CARTESIAN_POINT ( 'NONE',  ( -71.95000000000001705, 7.499999999999996447, 13.96446609406725514 ) ) ;
#13144 = CARTESIAN_POINT ( 'NONE',  ( -72.10000000109246798, 12.06698729999999919, 15.85617417291294196 ) ) ;
#13145 = EDGE_CURVE ( 'NONE', #20787, #12636, #6694, .T. ) ;
#13146 = CARTESIAN_POINT ( 'NONE',  ( -10.00000000000000000, 0.000000000000000000, 0.000000000000000000 ) ) ;
#13147 = ORIENTED_EDGE ( 'NONE', *, *, #11727, .F. ) ;
#13148 = FACE_OUTER_BOUND ( 'NONE', #14989, .T. ) ;
#13149 = DIRECTION ( 'NONE',  ( 0.000000000000000000, 0.000000000000000000, 1.000000000000000000 ) ) ;
#13150 = CARTESIAN_POINT ( 'NONE',  ( -20.00000000000000711, 4.500000000000003553, -19.99999999999999645 ) ) ;
#13151 = ORIENTED_EDGE ( 'NONE', *, *, #16881, .F. ) ;
#13152 = ORIENTED_EDGE ( 'NONE', *, *, #9243, .F. ) ;
#13153 = LINE ( 'NONE', #20539, #5251 ) ;
#13154 = EDGE_CURVE ( 'NONE', #2890, #14518, #6155, .T. ) ;
#13155 = CARTESIAN_POINT ( 'NONE',  ( 55.96875000000001421, 5.999999999999987566, 13.34314575050763452 ) ) ;
#13156 = ORIENTED_EDGE ( 'NONE', *, *, #15013, .T. ) ;
#13157 = LINE ( 'NONE', #902, #10694 ) ;
#13158 = EDGE_LOOP ( 'NONE', ( #1421, #15171, #3676, #12421 ) ) ;
#13159 = UNCERTAINTY_MEASURE_WITH_UNIT (LENGTH_MEASURE( 1.000000000000000082E-05 ), #21322, 'distance_accuracy_value', 'NONE');
#13160 = CARTESIAN_POINT ( 'NONE',  ( 52.25231816583844591, 7.219692298483957771, 17.87654654797633924 ) ) ;
#13161 = CARTESIAN_POINT ( 'NONE',  ( 65.90000000218495302, 11.76776695296636888, 13.23223304703362579 ) ) ;
#13162 = B_SPLINE_CURVE_WITH_KNOTS ( 'NONE', 3,
 ( #8529, #15833, #14028, #21291, #14867, #3931 ),
 .UNSPECIFIED., .F., .F.,
 ( 4, 2, 4 ),
 ( 0.01049192114530184301, 0.01239128608052813413, 0.01429065101575442351 ),
 .UNSPECIFIED. ) ;
#13163 = CARTESIAN_POINT ( 'NONE',  ( -3.999999999999999112, -2.265485919601331943, 20.08545885675730602 ) ) ;
#13164 = CARTESIAN_POINT ( 'NONE',  ( 9.546947090716562556, -8.974600000000002353, 5.000000000000079936 ) ) ;
#13165 = EDGE_LOOP ( 'NONE', ( #14665, #896, #7635, #5261 ) ) ;
#13166 = CARTESIAN_POINT ( 'NONE',  ( 1.656854249492384135, -3.999999999999999112, 13.43750000273119838 ) ) ;
#13167 = CARTESIAN_POINT ( 'NONE',  ( 4.999999999999999112, -0.4999240074893842034, -8.734705317681632053 ) ) ;
#13168 = CARTESIAN_POINT ( 'NONE',  ( 52.84143183416158251, 8.275094609562001935, 18.97181229448536044 ) ) ;
#13169 = CARTESIAN_POINT ( 'NONE',  ( 2.244686410773148566, -2.775871127258929594, 2.039999999999996927 ) ) ;
#13170 = FACE_OUTER_BOUND ( 'NONE', #19174, .T. ) ;
#13171 = FACE_OUTER_BOUND ( 'NONE', #9599, .T. ) ;
#13172 = ADVANCED_FACE ( 'NONE', ( #12105 ), #8973, .T. ) ;
#13173 = CARTESIAN_POINT ( 'NONE',  ( -66.90000000109247935, 7.933012699999995476, 14.14382582708705094 ) ) ;
#13174 = CARTESIAN_POINT ( 'NONE',  ( 20.55500000000001748, 0.000000000000000000, 0.000000000000000000 ) ) ;
#13175 = VERTEX_POINT ( 'NONE', #19819 ) ;
#13176 = CARTESIAN_POINT ( 'NONE',  ( 2.499999999999999556, 0.000000000000000000, 3.469446951953614189E-15 ) ) ;
#13177 = ADVANCED_FACE ( 'NONE', ( #5097 ), #23419, .F. ) ;
#13178 = CARTESIAN_POINT ( 'NONE',  ( 52.03125000000000711, 11.24264068711929276, 18.00000000000000000 ) ) ;
#13179 = CARTESIAN_POINT ( 'NONE',  ( -10.00000000000000000, 0.000000000000000000, 0.000000000000000000 ) ) ;
#13180 = PRESENTATION_STYLE_ASSIGNMENT (( #12944 ) ) ;
#13181 = ORIENTED_EDGE ( 'NONE', *, *, #21829, .T. ) ;
#13182 = CARTESIAN_POINT ( 'NONE',  ( -65.97500000054623115, 9.999999999999998224, 17.28349365000000049 ) ) ;
#13183 = CARTESIAN_POINT ( 'NONE',  ( 70.84999999999998010, 11.03553390593276973, 17.49999999999997158 ) ) ;
#13184 = DIRECTION ( 'NONE',  ( -1.000000000000000000, 0.000000000000000000, 1.224646799147353207E-16 ) ) ;
#13185 = EDGE_CURVE ( 'NONE', #8728, #17247, #17690, .T. ) ;
#13186 = LINE ( 'NONE', #7109, #17893 ) ;
#13187 = ORIENTED_EDGE ( 'NONE', *, *, #14094, .F. ) ;
#13188 = DIRECTION ( 'NONE',  ( 0.000000000000000000, 0.000000000000000000, -1.000000000000000000 ) ) ;
#13189 = ORIENTED_EDGE ( 'NONE', *, *, #3034, .F. ) ;
#13190 = EDGE_CURVE ( 'NONE', #12546, #2635, #21681, .T. ) ;
#13191 = DIRECTION ( 'NONE',  ( 0.8191520442889875797, 0.000000000000000000, 0.5735764363510522656 ) ) ;
#13192 = CARTESIAN_POINT ( 'NONE',  ( -3.999999999999999112, 1.656854249492380804, 15.93750000000001066 ) ) ;
#13193 = DIRECTION ( 'NONE',  ( 0.000000000000000000, 0.000000000000000000, 1.000000000000000000 ) ) ;
#13194 = FACE_OUTER_BOUND ( 'NONE', #6952, .T. ) ;
#13195 = CARTESIAN_POINT ( 'NONE',  ( 71.40000000109246514, 10.85617417291294551, 17.06698730000000097 ) ) ;
#13196 = ORIENTED_EDGE ( 'NONE', *, *, #2620, .F. ) ;
#13197 = CARTESIAN_POINT ( 'NONE',  ( -4.000000000000000000, 2.309401076758498483, -5.000000000000000000 ) ) ;
#13198 = VECTOR ( 'NONE', #13475, 1000.000000000000114 ) ;
#13199 = EDGE_CURVE ( 'NONE', #8748, #3547, #3537, .T. ) ;
#13200 = CARTESIAN_POINT ( 'NONE',  ( 66.20000000218495018, 9.999999999999998224, 17.49999999999999645 ) ) ;
#13201 = CARTESIAN_POINT ( 'NONE',  ( 66.55000000109247082, 8.538419263543522320, 16.46158073645647235 ) ) ;
#13202 = CARTESIAN_POINT ( 'NONE',  ( -1.432654583217639610, -3.458734124999999882, 18.62500000136560274 ) ) ;
#13203 = DIRECTION ( 'NONE',  ( -1.000000000000000000, -0.000000000000000000, -0.000000000000000000 ) ) ;
#13204 = CARTESIAN_POINT ( 'NONE',  ( 2.445694354108820079, 2.445694354108820523, -1.387499998634402987 ) ) ;
#13205 = CARTESIAN_POINT ( 'NONE',  ( -4.000000000000000000, 0.000000000000000000, 0.3000000000000016542 ) ) ;
#13206 = EDGE_CURVE ( 'NONE', #21976, #6753, #1419, .T. ) ;
#13207 = DIRECTION ( 'NONE',  ( 0.000000000000000000, 0.000000000000000000, 1.000000000000000000 ) ) ;
#13208 = CARTESIAN_POINT ( 'NONE',  ( 3.458734125000001214, 1.432654583217640498, 13.00000000136560452 ) ) ;
#13209 = LINE ( 'NONE', #11896, #10371 ) ;
#13210 = VERTEX_POINT ( 'NONE', #19468 ) ;
#13211 = CARTESIAN_POINT ( 'NONE',  ( -69.80000000109247082, 7.933012699999995476, 15.85617417291294196 ) ) ;
#13212 = ORIENTED_EDGE ( 'NONE', *, *, #1201, .T. ) ;
#13213 = CARTESIAN_POINT ( 'NONE',  ( 56.81250000000000000, 14.00000000000000000, 14.99999999999997691 ) ) ;
#13214 = CARTESIAN_POINT ( 'NONE',  ( -71.00000000109245946, 9.143825827087050939, 12.93301269999999370 ) ) ;
#13215 = PRODUCT_CONTEXT ( 'NONE', #9014, 'mechanical' ) ;
#13216 = EDGE_CURVE ( 'NONE', #3172, #16212, #17917, .T. ) ;
#13217 = ORIENTED_EDGE ( 'NONE', *, *, #16570, .T. ) ;
#13218 = CARTESIAN_POINT ( 'NONE',  ( -20.00000000000001066, 9.999999999999964473, -49.99999999999999289 ) ) ;
#13219 = VERTEX_POINT ( 'NONE', #23537 ) ;
#13220 = EDGE_CURVE ( 'NONE', #21260, #10183, #22833, .T. ) ;
#13221 = VERTEX_POINT ( 'NONE', #10410 ) ;
#13222 = CARTESIAN_POINT ( 'NONE',  ( -1.432654583217639832, -3.458734125000000326, 18.87500000136560274 ) ) ;
#13223 = CARTESIAN_POINT ( 'NONE',  ( 55.31250000000000711, 13.00000000000000000, 14.99999999999998757 ) ) ;
#13224 = VECTOR ( 'NONE', #7161, 1000.000000000000000 ) ;
#13225 = AXIS2_PLACEMENT_3D ( 'NONE', #12948, #19866, #12831 ) ;
#13226 = CARTESIAN_POINT ( 'NONE',  ( -68.15000000109247935, 8.538419263543522320, 16.46158073645647235 ) ) ;
#13227 = CIRCLE ( 'NONE', #12846, 2.649999999999999467 ) ;
#13228 = CARTESIAN_POINT ( 'NONE',  ( 68.40000000109249356, 9.143825827087052716, 12.93301269999999192 ) ) ;
#13229 = CARTESIAN_POINT ( 'NONE',  ( -66.90000000109246514, 7.933012699999995476, 14.14382582708705094 ) ) ;
#13230 = CARTESIAN_POINT ( 'NONE',  ( 6.499999999999999112, -3.752776749732574135, -0.5805565836007695601 ) ) ;
#13231 = CARTESIAN_POINT ( 'NONE',  ( 59.40393183416158251, 13.02818770551463778, 13.82541045382633982 ) ) ;
#13232 = CARTESIAN_POINT ( 'NONE',  ( -0.3649867057748917842, 3.983313282257320509, 9.889028792932920808 ) ) ;
#13233 =( BOUNDED_CURVE ( )  B_SPLINE_CURVE ( 2, ( #19837, #19489, #3087, #6805, #5010, #3198, #17821, #1387, #8727, #23323, #1982, #8982, #3554, #20302, #11362, #192, #16270, #9321, #4027, #18405, #3787, #18637, #20064, #16383, #12918, #16613, #23562, #14485, #7522, #2099, #20417, #7168, #7296, #12702, #21747, #5359, #14837, #10891, #5592, #22093, #9215, #19955, #18170, #13155, #1753, #9089, #14605, #5710, #3904, #11238, #23680, #21977, #13042, #5828, #7409, #18513, #9437, #11127, #5471, #16729, #312, #11002, #21866, #12807, #3667, #1867, #18284, #16500, #7646, #14964, #75, #14719, #20181, #22217, #10046, #9795, #11721, #18989, #2224, #20541, #13628, #21011, #11608, #22699, #4271, #2575, #17334, #6429, #4628, #13400, #9680, #6194, #9921, #9565, #7760, #17217, #19116 ),
 .UNSPECIFIED., .F., .F. ) 
 B_SPLINE_CURVE_WITH_KNOTS ( ( 3, 2, 2, 2, 2, 2, 2, 2, 2, 2, 2, 2, 2, 2, 2, 2, 2, 2, 2, 2, 2, 2, 2, 2, 2, 2, 2, 2, 2, 2, 2, 2, 2, 2, 2, 2, 2, 2, 2, 2, 2, 2, 2, 2, 2, 2, 2, 2, 3 ),
 ( 0.000000000000000000, 0.02083333333333333218, 0.04166666666666666435, 0.06250000000000000000, 0.08333333333333332871, 0.1041666666666666713, 0.1250000000000000000, 0.1458333333333333426, 0.1666666666666666574, 0.1875000000000000000, 0.2083333333333333426, 0.2291666666666666574, 0.2500000000000000000, 0.2708333333333333148, 0.2916666666666666852, 0.3125000000000000000, 0.3333333333333333148, 0.3541666666666666852, 0.3750000000000000000, 0.3958333333333333148, 0.4166666666666666852, 0.4375000000000000000, 0.4583333333333333148, 0.4791666666666666852, 0.5000000000000000000, 0.5208333333333333703, 0.5416666666666666297, 0.5625000000000000000, 0.5833333333333333703, 0.6041666666666666297, 0.6250000000000000000, 0.6458333333333333703, 0.6666666666666666297, 0.6875000000000000000, 0.7083333333333333703, 0.7291666666666666297, 0.7500000000000000000, 0.7708333333333333703, 0.7916666666666666297, 0.8125000000000000000, 0.8333333333333333703, 0.8541666666666666297, 0.8750000000000000000, 0.8958333333333333703, 0.9166666666666666297, 0.9375000000000000000, 0.9583333333333333703, 0.9791666666666666297, 1.000000000000000000 ),
 .UNSPECIFIED. ) 
 CURVE ( )  GEOMETRIC_REPRESENTATION_ITEM ( )  RATIONAL_B_SPLINE_CURVE ( ( 1.000000000000000000, 0.9238795325112867385, 1.000000000000000000, 0.9238795325112867385, 1.000000000000000000, 0.9238795325112867385, 1.000000000000000000, 0.9238795325112867385, 1.000000000000000000, 0.9238795325112867385, 1.000000000000000000, 0.9238795325112867385, 1.000000000000000000, 0.9238795325112867385, 1.000000000000000000, 0.9238795325112867385, 1.000000000000000000, 0.9238795325112867385, 1.000000000000000000, 0.9238795325112867385, 1.000000000000000000, 0.9238795325112867385, 1.000000000000000000, 0.9238795325112867385, 1.000000000000000000, 0.9238795325112867385, 1.000000000000000000, 0.9238795325112867385, 1.000000000000000000, 0.9238795325112867385, 1.000000000000000000, 0.9238795325112867385, 1.000000000000000000, 0.9238795325112867385, 1.000000000000000000, 0.9238795325112867385, 1.000000000000000000, 0.9238795325112867385, 1.000000000000000000, 0.9238795325112867385, 1.000000000000000000, 0.9238795325112867385, 1.000000000000000000, 0.9238795325112867385, 1.000000000000000000, 0.9238795325112867385, 1.000000000000000000, 0.9238795325112867385, 1.000000000000000000, 0.9238795325112867385, 1.000000000000000000, 0.9238795325112867385, 1.000000000000000000, 0.9238795325112867385, 1.000000000000000000, 0.9238795325112867385, 1.000000000000000000, 0.9238795325112867385, 1.000000000000000000, 0.9238795325112867385, 1.000000000000000000, 0.9238795325112867385, 1.000000000000000000, 0.9238795325112867385, 1.000000000000000000, 0.9238795325112867385, 1.000000000000000000, 0.9238795325112867385, 1.000000000000000000, 0.9238795325112867385, 1.000000000000000000, 0.9238795325112867385, 1.000000000000000000, 0.9238795325112867385, 1.000000000000000000, 0.9238795325112867385, 1.000000000000000000, 0.9238795325112867385, 1.000000000000000000, 0.9238795325112867385, 1.000000000000000000, 0.9238795325112867385, 1.000000000000000000, 0.9238795325112867385, 1.000000000000000000, 0.9238795325112867385, 1.000000000000000000, 0.9238795325112867385, 1.000000000000000000, 0.9238795325112867385, 1.000000000000000000, 0.9238795325112867385, 1.000000000000000000, 0.9238795325112867385, 1.000000000000000000, 0.9238795325112867385, 1.000000000000000000 ) ) 
 REPRESENTATION_ITEM ( '' )  );
#13234 = CARTESIAN_POINT ( 'NONE',  ( 3.458734125000000770, 1.432654583217640498, 2.550000001365598123 ) ) ;
#13235 = LINE ( 'NONE', #10002, #10522 ) ;
#13236 = CARTESIAN_POINT ( 'NONE',  ( 1.971781867644420635E-15, -4.000000000000000000, 15.37500000273119660 ) ) ;
#13237 = DIRECTION ( 'NONE',  ( -1.224646799147353207E-16, 0.000000000000000000, -1.000000000000000000 ) ) ;
#13238 = VERTEX_POINT ( 'NONE', #21368 ) ;
#13239 = DIRECTION ( 'NONE',  ( -0.000000000000000000, -0.000000000000000000, -1.000000000000000000 ) ) ;
#13240 = VERTEX_POINT ( 'NONE', #10523 ) ;
#13241 = CARTESIAN_POINT ( 'NONE',  ( 59.49768183416157541, 12.16943976678977535, 12.92679907967048614 ) ) ;
#13242 = VECTOR ( 'NONE', #7611, 1000.000000000000000 ) ;
#13243 = FILL_AREA_STYLE_COLOUR ( '', #17547 ) ;
#13244 = CARTESIAN_POINT ( 'NONE',  ( 3.458734125000000326, 4.235727675282971730E-16, 1.237500001365595903 ) ) ;
#13245 = VECTOR ( 'NONE', #3434, 1000.000000000000000 ) ;
#13246 = EDGE_CURVE ( 'NONE', #16324, #16789, #14253, .T. ) ;
#13247 = CARTESIAN_POINT ( 'NONE',  ( 4.000000000000000888, 4.898587196589412829E-16, 21.31370849898476649 ) ) ;
#13248 = EDGE_LOOP ( 'NONE', ( #11084, #15191, #16610, #5549 ) ) ;
#13249 = CARTESIAN_POINT ( 'NONE',  ( 2.828427124746191179, 2.828427124746190291, 11.62500000000001066 ) ) ;
#13250 = EDGE_CURVE ( 'NONE', #6771, #1981, #12556, .T. ) ;
#13251 = CARTESIAN_POINT ( 'NONE',  ( 36.99310306966726358, -11.25000000000000355, 5.000000000000079936 ) ) ;
#13252 = CARTESIAN_POINT ( 'NONE',  ( 4.000000000000000888, 4.898587196589412829E-16, 14.50000000000001066 ) ) ;
#13253 = ORIENTED_EDGE ( 'NONE', *, *, #3924, .F. ) ;
#13254 = VECTOR ( 'NONE', #2375, 1000.000000000000000 ) ;
#13255 = CIRCLE ( 'NONE', #15173, 2.055000000000000160 ) ;
#13256 = CARTESIAN_POINT ( 'NONE',  ( -70.25000000218494733, 8.964466094067258695, 17.50000000000000355 ) ) ;
#13257 = CARTESIAN_POINT ( 'NONE',  ( -3.458734125000000770, 0.000000000000000000, 0.9875000013655956810 ) ) ;
#13258 = TOROIDAL_SURFACE ( 'NONE', #2119, 6.760799999999997034, 0.03079999999999879709 ) ;
#13259 = CARTESIAN_POINT ( 'NONE',  ( 67.20000000000000284, 8.232233047033629347, 13.23223304703362402 ) ) ;
#13260 = CARTESIAN_POINT ( 'NONE',  ( -71.14999999999999147, 7.499999999999996447, 13.96446609406725514 ) ) ;
#13261 = CARTESIAN_POINT ( 'NONE',  ( 50.37731816583844591, 7.123453452023657206, 12.21969229848395599 ) ) ;
#13262 = CARTESIAN_POINT ( 'NONE',  ( 1.432654583217642275, -3.458734124999999882, 4.300000001365595459 ) ) ;
#13263 = CARTESIAN_POINT ( 'NONE',  ( 3.458734125000001658, 1.432654583217640498, 16.25000000136560629 ) ) ;
#13264 = CARTESIAN_POINT ( 'NONE',  ( 68.70000000218495018, 8.232233047033627571, 16.76776695296636532 ) ) ;
#13265 = CARTESIAN_POINT ( 'NONE',  ( 0.000000000000000000, 8.264486777890107660, 4.472189673936815879 ) ) ;
#13266 = CARTESIAN_POINT ( 'NONE',  ( -69.89999999999999147, 12.50000000000000000, 14.99999999999999645 ) ) ;
#13267 = VERTEX_POINT ( 'NONE', #5340 ) ;
#13268 = FACE_OUTER_BOUND ( 'NONE', #4143, .T. ) ;
#13269 = CYLINDRICAL_SURFACE ( 'NONE', #22104, 2.499999999999998668 ) ;
#13270 = CARTESIAN_POINT ( 'NONE',  ( 0.000000000000000000, 9.680994141368771011, 5.222868219166890036 ) ) ;
#13271 = ORIENTED_EDGE ( 'NONE', *, *, #4767, .T. ) ;
#13272 = VERTEX_POINT ( 'NONE', #16361 ) ;
#13273 = DIRECTION ( 'NONE',  ( -1.000000000000000000, -0.000000000000000000, -0.000000000000000000 ) ) ;
#13274 = DIRECTION ( 'NONE',  ( -0.000000000000000000, -0.000000000000000000, -1.000000000000000000 ) ) ;
#13275 = ORIENTED_EDGE ( 'NONE', *, *, #3074, .F. ) ;
#13276 = CARTESIAN_POINT ( 'NONE',  ( -13.27237933033274153, -11.25000000000000355, 10.00000000000008882 ) ) ;
#13277 = ORIENTED_EDGE ( 'NONE', *, *, #22492, .T. ) ;
#13278 = CARTESIAN_POINT ( 'NONE',  ( 53.28356816583845301, 8.275094609561968184, 11.02818770551464667 ) ) ;
#13279 = CARTESIAN_POINT ( 'NONE',  ( 70.85000000109246798, 9.999999999999998224, 12.93301269999999192 ) ) ;
#13280 = ADVANCED_FACE ( 'NONE', ( #13984 ), #1033, .T. ) ;
#13281 = DIRECTION ( 'NONE',  ( -1.000000000000000000, -0.000000000000000000, -0.000000000000000000 ) ) ;
#13282 = ORIENTED_EDGE ( 'NONE', *, *, #14094, .T. ) ;
#13283 = DIRECTION ( 'NONE',  ( 1.000000000000000000, 7.703719777548943412E-32, 0.000000000000000000 ) ) ;
#13284 = EDGE_LOOP ( 'NONE', ( #5392, #22451, #16776, #17005 ) ) ;
#13285 = CARTESIAN_POINT ( 'NONE',  ( -1.656854249492379250, 4.000000000000000000, 12.93750000273119660 ) ) ;
#13286 = AXIS2_PLACEMENT_3D ( 'NONE', #5044, #19641, #17748 ) ;
#13287 = CARTESIAN_POINT ( 'NONE',  ( 27.50000000000000000, 1.500000000000003109, -33.66025403784446723 ) ) ;
#13288 = CARTESIAN_POINT ( 'NONE',  ( 52.74768183416157541, 7.123453452023678523, 17.78030770151605822 ) ) ;
#13289 = DIRECTION ( 'NONE',  ( 1.000000000000000000, 0.000000000000000000, 0.000000000000000000 ) ) ;
#13290 = DIRECTION ( 'NONE',  ( -0.000000000000000000, -1.000000000000000000, -0.000000000000000000 ) ) ;
#13291 = CARTESIAN_POINT ( 'NONE',  ( 4.000000000000000000, 4.898587196589412829E-16, 0.8000000000000020428 ) ) ;
#13292 = CARTESIAN_POINT ( 'NONE',  ( 4.000000000000000000, -0.8732470631449981147, -3.223155494240760088 ) ) ;
#13293 = ORIENTED_EDGE ( 'NONE', *, *, #23465, .T. ) ;
#13294 = CARTESIAN_POINT ( 'NONE',  ( 53.71875000000000711, 13.00000000000000533, 16.24264068711927322 ) ) ;
#13295 = DIRECTION ( 'NONE',  ( 0.000000000000000000, -0.8090169943749532244, 0.5877852522924652545 ) ) ;
#13296 = VECTOR ( 'NONE', #17746, 1000.000000000000000 ) ;
#13297 = EDGE_LOOP ( 'NONE', ( #12836, #21480, #3018, #8118 ) ) ;
#13298 = DIRECTION ( 'NONE',  ( 0.000000000000000000, 0.000000000000000000, 1.000000000000000000 ) ) ;
#13299 = CARTESIAN_POINT ( 'NONE',  ( 23.53786173033275375, -11.25000000000000355, 5.000000000000079936 ) ) ;
#13300 = FACE_OUTER_BOUND ( 'NONE', #8950, .T. ) ;
#13301 = CARTESIAN_POINT ( 'NONE',  ( 2.500000000000000000, -2.357898499370432166, 3.035766082959412415E-15 ) ) ;
#13302 = ORIENTED_EDGE ( 'NONE', *, *, #9725, .T. ) ;
#13303 = CARTESIAN_POINT ( 'NONE',  ( 3.250000000000003109, 5.629165124598848102, 1.734723475976807094E-15 ) ) ;
#13304 = ORIENTED_EDGE ( 'NONE', *, *, #11465, .F. ) ;
#13305 = DIRECTION ( 'NONE',  ( 0.000000000000000000, 0.000000000000000000, -1.000000000000000000 ) ) ;
#13306 = CARTESIAN_POINT ( 'NONE',  ( -3.999999999999998224, -1.656854249492383246, 13.06250000000001066 ) ) ;
#13307 = DIRECTION ( 'NONE',  ( 0.000000000000000000, -1.000000000000000000, 1.287488025362403787E-15 ) ) ;
#13308 = AXIS2_PLACEMENT_3D ( 'NONE', #8590, #14105, #12318 ) ;
#13309 = EDGE_CURVE ( 'NONE', #7048, #16373, #10638, .T. ) ;
#13310 = CARTESIAN_POINT ( 'NONE',  ( 2.696295709017754838, 5.948846446048901448, -3.700000000000005063 ) ) ;
#13311 = ADVANCED_FACE ( 'NONE', ( #2327 ), #18613, .T. ) ;
#13312 = CARTESIAN_POINT ( 'NONE',  ( 72.50000000000000000, 9.999999999999998224, 17.49999999999999645 ) ) ;
#13313 = CARTESIAN_POINT ( 'NONE',  ( 70.05000000109247082, 7.933012699999995476, 14.99999999999999645 ) ) ;
#13314 = ORIENTED_EDGE ( 'NONE', *, *, #8082, .F. ) ;
#13315 = AXIS2_PLACEMENT_3D ( 'NONE', #8951, #19573, #17683 ) ;
#13316 = AXIS2_PLACEMENT_3D ( 'NONE', #14249, #10662, #21150 ) ;
#13317 = CARTESIAN_POINT ( 'NONE',  ( 48.67060293033276963, -11.25000000000000355, 10.00000000000008882 ) ) ;
#13318 = DIRECTION ( 'NONE',  ( 0.000000000000000000, 0.000000000000000000, -1.000000000000000000 ) ) ;
#13319 = EDGE_CURVE ( 'NONE', #1325, #15816, #12468, .T. ) ;
#13320 = CARTESIAN_POINT ( 'NONE',  ( 67.20000000109247651, 10.85617417291294551, 17.06698729999999742 ) ) ;
#13321 = CARTESIAN_POINT ( 'NONE',  ( -3.458734124999998993, 1.432654583217640276, 13.37500000136560452 ) ) ;
#13322 = CARTESIAN_POINT ( 'NONE',  ( -55.00000000000000000, 15.00000000000000000, 10.00000000000001599 ) ) ;
#13323 = CARTESIAN_POINT ( 'NONE',  ( 2.445694354108820967, -2.445694354108820079, -1.637499998634403209 ) ) ;
#13324 = CARTESIAN_POINT ( 'NONE',  ( 4.000000000000000888, -1.656854249492379694, 1.737500000000001377 ) ) ;
#13325 = LINE ( 'NONE', #20594, #8648 ) ;
#13326 = DIRECTION ( 'NONE',  ( 0.000000000000000000, -1.000000000000000000, 0.000000000000000000 ) ) ;
#13327 = DIRECTION ( 'NONE',  ( -0.000000000000000000, 0.000000000000000000, -1.000000000000000000 ) ) ;
#13328 = ORIENTED_EDGE ( 'NONE', *, *, #5158, .T. ) ;
#13329 = CIRCLE ( 'NONE', #19406, 2.500000000000007550 ) ;
#13330 = CARTESIAN_POINT ( 'NONE',  ( -66.95000000109246230, 11.46158073645647235, 13.53841926354352232 ) ) ;
#13331 = ORIENTED_EDGE ( 'NONE', *, *, #16314, .F. ) ;
#13332 = CARTESIAN_POINT ( 'NONE',  ( 57.75000000000000000, 7.171572875253819923, 17.82842712474619873 ) ) ;
#13333 = CARTESIAN_POINT ( 'NONE',  ( -70.65000000109246514, 9.999999999999998224, 17.06698730000000097 ) ) ;
#13334 = ITEM_DEFINED_TRANSFORMATION ( 'NONE', 'NONE', #19435,  #7318 ) ;
#13335 = ORIENTED_EDGE ( 'NONE', *, *, #22427, .F. ) ;
#13336 = DIRECTION ( 'NONE',  ( -1.000000000000000000, -0.000000000000000000, -0.000000000000000000 ) ) ;
#13337 = ORIENTED_EDGE ( 'NONE', *, *, #2604, .F. ) ;
#13338 = CIRCLE ( 'NONE', #2969, 2.500000000000000444 ) ;
#13339 = VECTOR ( 'NONE', #9656, 1000.000000000000000 ) ;
#13340 = ORIENTED_EDGE ( 'NONE', *, *, #22661, .F. ) ;
#13341 = CARTESIAN_POINT ( 'NONE',  ( 1.025207404391860050E-15, 3.458734125000000770, 17.43750000136560274 ) ) ;
#13342 = CARTESIAN_POINT ( 'NONE',  ( 57.46875000000000711, 6.999999999999992895, 13.75735931288071967 ) ) ;
#13343 = CARTESIAN_POINT ( 'NONE',  ( -67.40000000109247935, 7.933012699999995476, 15.85617417291294196 ) ) ;
#13344 = ADVANCED_FACE ( 'NONE', ( #15293 ), #13374, .T. ) ;
#13345 = CARTESIAN_POINT ( 'NONE',  ( 67.65000000109247935, 9.999999999999998224, 12.93301269999999192 ) ) ;
#13346 = VECTOR ( 'NONE', #22887, 1000.000000000000000 ) ;
#13347 = CARTESIAN_POINT ( 'NONE',  ( -65.95000000109246230, 8.538419263543522320, 16.46158073645647235 ) ) ;
#13348 = DIRECTION ( 'NONE',  ( 0.000000000000000000, 0.000000000000000000, 1.000000000000000000 ) ) ;
#13349 = EDGE_CURVE ( 'NONE', #10047, #6314, #4251, .T. ) ;
#13350 = CARTESIAN_POINT ( 'NONE',  ( 54.90393183416157541, 13.02818770551463778, 13.82541045382633982 ) ) ;
#13351 = FACE_OUTER_BOUND ( 'NONE', #4300, .T. ) ;
#13352 = AXIS2_PLACEMENT_3D ( 'NONE', #4826, #12157, #17537 ) ;
#13353 = EDGE_CURVE ( 'NONE', #17879, #16821, #19316, .T. ) ;
#13354 = CARTESIAN_POINT ( 'NONE',  ( 2.445694354108820079, 2.445694354108820523, 2.612500001365597235 ) ) ;
#13355 = CARTESIAN_POINT ( 'NONE',  ( 46.41788101966725577, -11.25000000000000355, 10.00000000000008882 ) ) ;
#13356 = CARTESIAN_POINT ( 'NONE',  ( -3.999999999999999112, 1.656854249492380804, 17.06250000273120193 ) ) ;
#13357 = CARTESIAN_POINT ( 'NONE',  ( -69.40000000218495302, 9.999999999999998224, 17.49999999999999645 ) ) ;
#13358 = ORIENTED_EDGE ( 'NONE', *, *, #2436, .F. ) ;
#13359 = CARTESIAN_POINT ( 'NONE',  ( 2.828427124746191179, 2.828427124746190291, 13.62500000000001066 ) ) ;
#13360 = ORIENTED_EDGE ( 'NONE', *, *, #10568, .F. ) ;
#13361 = CARTESIAN_POINT ( 'NONE',  ( 56.12268183416157541, 12.07320092032950676, 17.16943976678977180 ) ) ;
#13362 = CARTESIAN_POINT ( 'NONE',  ( 3.458734125000000326, 1.432654583217640498, 1.300000001365597235 ) ) ;
#13363 = AXIS2_PLACEMENT_3D ( 'NONE', #2880, #11793, #17046 ) ;
#13364 = LINE ( 'NONE', #11577, #5570 ) ;
#13365 = EDGE_LOOP ( 'NONE', ( #20251, #3377, #4788, #12725 ) ) ;
#13366 = CARTESIAN_POINT ( 'NONE',  ( -2.828427124746188515, -2.828427124746190735, 12.12500000000001066 ) ) ;
#13367 = CIRCLE ( 'NONE', #23661, 11.00000000000000000 ) ;
#13368 = CARTESIAN_POINT ( 'NONE',  ( 0.000000000000000000, 0.000000000000000000, -3.699999999999998401 ) ) ;
#13369 = CARTESIAN_POINT ( 'NONE',  ( 60.00000000000000711, 12.47487373415290612, 12.52512626584706901 ) ) ;
#13370 = ORIENTED_EDGE ( 'NONE', *, *, #9295, .F. ) ;
#13371 = PRODUCT_DEFINITION_SHAPE ( 'NONE', 'NONE',  #23711 ) ;
#13372 = CARTESIAN_POINT ( 'NONE',  ( -69.70000000218495018, 8.232233047033629347, 13.23223304703362402 ) ) ;
#13373 = CIRCLE ( 'NONE', #19830, 4.000000000000001776 ) ;
#13374 = CYLINDRICAL_SURFACE ( 'NONE', #13688, 4.000000000000000000 ) ;
#13375 = DIRECTION ( 'NONE',  ( 0.000000000000000000, 0.000000000000000000, 1.000000000000000000 ) ) ;
#13376 = EDGE_CURVE ( 'NONE', #17685, #14695, #17192, .T. ) ;
#13377 = CARTESIAN_POINT ( 'NONE',  ( 67.95000000000000284, 7.499999999999995559, 13.96446609406725692 ) ) ;
#13379 = EDGE_CURVE ( 'NONE', #17245, #7757, #7974, .T. ) ;
#13378 = CIRCLE ( 'NONE', #19467, 6.500000000000000888 ) ;
#13380 = DIRECTION ( 'NONE',  ( 0.3420201433256622181, 0.9396926207859107594, -6.162975822039141593E-32 ) ) ;
#13381 = EDGE_CURVE ( 'NONE', #6601, #18050, #15527, .T. ) ;
#13382 = AXIS2_PLACEMENT_3D ( 'NONE', #15203, #18997, #16872 ) ;
#13383 = CARTESIAN_POINT ( 'NONE',  ( -67.09999999999999432, 7.499999999999996447, 14.99999999999999645 ) ) ;
#13384 = CARTESIAN_POINT ( 'NONE',  ( 55.15856816583844591, 7.028187705514647554, 16.31069182806492179 ) ) ;
#13385 = CARTESIAN_POINT ( 'NONE',  ( 2.445694354108820079, 2.445694354108820523, -2.637499998634404097 ) ) ;
#13386 = CARTESIAN_POINT ( 'NONE',  ( -2.445694354108818303, -2.445694354108820967, 15.81250000136560629 ) ) ;
#13387 = LINE ( 'NONE', #9783, #3428 ) ;
#13388 = CARTESIAN_POINT ( 'NONE',  ( -70.30000000109247082, 10.85617417291294551, 12.93301269999999192 ) ) ;
#13389 = CARTESIAN_POINT ( 'NONE',  ( 58.50000000000000000, 12.12132034355963484, 12.87867965644034740 ) ) ;
#13390 = COLOUR_RGB ( '', 0.09019608, 0.27058824, 0.51372549) ;
#13391 = LINE ( 'NONE', #16720, #1734 ) ;
#13392 = VERTEX_POINT ( 'NONE', #13494 ) ;
#13393 = CARTESIAN_POINT ( 'NONE',  ( -1.360585162435467455, 4.061296242128285883, -3.505054077164959203 ) ) ;
#13394 = CARTESIAN_POINT ( 'NONE',  ( 4.000000000000000000, 1.656854249492381248, 4.987500002731185766 ) ) ;
#13395 = CARTESIAN_POINT ( 'NONE',  ( -70.00000000109248788, 9.143825827087050939, 12.93301269999999370 ) ) ;
#13396 = ORIENTED_EDGE ( 'NONE', *, *, #2896, .F. ) ;
#13397 = EDGE_LOOP ( 'NONE', ( #2931, #4535, #10240, #13302 ) ) ;
#13398 = DIRECTION ( 'NONE',  ( 0.000000000000000000, 0.000000000000000000, 1.000000000000000000 ) ) ;
#13399 = AXIS2_PLACEMENT_3D ( 'NONE', #22623, #19026, #9606 ) ;
#13400 = CARTESIAN_POINT ( 'NONE',  ( 51.65625000000000711, 6.000000000000004441, 16.65685424949239390 ) ) ;
#13401 = ORIENTED_EDGE ( 'NONE', *, *, #18037, .T. ) ;
#13402 = DIRECTION ( 'NONE',  ( 0.000000000000000000, 0.000000000000000000, -1.000000000000000000 ) ) ;
#13403 = AXIS2_PLACEMENT_3D ( 'NONE', #5217, #20523, #22438 ) ;
#13404 = CARTESIAN_POINT ( 'NONE',  ( 69.55000000109247082, 11.46158073645647235, 16.46158073645647235 ) ) ;
#13405 = LINE ( 'NONE', #20425, #3 ) ;
#13406 = EDGE_CURVE ( 'NONE', #4376, #15000, #20754, .T. ) ;
#13407 = CARTESIAN_POINT ( 'NONE',  ( 70.95000000109247651, 8.538419263543524096, 13.53841926354352054 ) ) ;
#13408 = ORIENTED_EDGE ( 'NONE', *, *, #10568, .T. ) ;
#13409 = CARTESIAN_POINT ( 'NONE',  ( -1.656854249492379250, 4.000000000000000000, 11.93750000273119660 ) ) ;
#13410 = DIRECTION ( 'NONE',  ( -1.000000000000000000, 0.000000000000000000, -0.000000000000000000 ) ) ;
#13411 = CARTESIAN_POINT ( 'NONE',  ( 54.65625000000001421, 6.000000000000004441, 16.65685424949239390 ) ) ;
#13412 = DIRECTION ( 'NONE',  ( -0.3420201433256622181, 0.9396926207859106484, 1.232595164407828100E-31 ) ) ;
#13413 = CARTESIAN_POINT ( 'NONE',  ( 66.60000000218495586, 9.999999999999998224, 12.49999999999999289 ) ) ;
#13414 = AXIS2_PLACEMENT_3D ( 'NONE', #5719, #13281, #3910 ) ;
#13415 = DIRECTION ( 'NONE',  ( 1.000000000000000000, 0.000000000000000000, -0.000000000000000000 ) ) ;
#13416 = VECTOR ( 'NONE', #2029, 1000.000000000000000 ) ;
#13417 = DIRECTION ( 'NONE',  ( 1.000000000000000000, -0.000000000000000000, -0.000000000000000000 ) ) ;
#13418 = VERTEX_POINT ( 'NONE', #4718 ) ;
#13419 = FACE_OUTER_BOUND ( 'NONE', #23357, .T. ) ;
#13420 = VERTEX_POINT ( 'NONE', #20987 ) ;
#13421 = DIRECTION ( 'NONE',  ( 1.000000000000000000, -0.000000000000000000, -0.000000000000000000 ) ) ;
#13422 = FACE_OUTER_BOUND ( 'NONE', #23345, .T. ) ;
#13423 = AXIS2_PLACEMENT_3D ( 'NONE', #7402, #7636, #14959 ) ;
#13424 = VERTEX_POINT ( 'NONE', #4606 ) ;
#13425 = CARTESIAN_POINT ( 'NONE',  ( 69.40000000218495302, 9.999999999999998224, 17.49999999999999645 ) ) ;
#13426 = CARTESIAN_POINT ( 'NONE',  ( 14.99999999999995559, 15.00000000000000000, -50.00000000000000000 ) ) ;
#13427 = DIRECTION ( 'NONE',  ( 0.000000000000000000, -0.8090169943749532244, 0.5877852522924653655 ) ) ;
#13428 = VECTOR ( 'NONE', #6977, 1000.000000000000000 ) ;
#13429 = CARTESIAN_POINT ( 'NONE',  ( 0.000000000000000000, -8.461683424509299556, -2.223716399045660097 ) ) ;
#13430 = ORIENTED_EDGE ( 'NONE', *, *, #11296, .F. ) ;
#13431 = LINE ( 'NONE', #2256, #12229 ) ;
#13432 = ORIENTED_EDGE ( 'NONE', *, *, #2865, .F. ) ;
#13433 = CARTESIAN_POINT ( 'NONE',  ( 71.45000000109247651, 7.933012699999995476, 14.99999999999999645 ) ) ;
#13434 = B_SPLINE_CURVE_WITH_KNOTS ( 'NONE', 3,
 ( #18337, #16781, #12850, #14534, #21673, #5282 ),
 .UNSPECIFIED., .F., .F.,
 ( 4, 2, 4 ),
 ( 0.002452478801916361129, 0.003676905084148001344, 0.004901331366379641126 ),
 .UNSPECIFIED. ) ;
#13435 = CARTESIAN_POINT ( 'NONE',  ( 2.828427124746191179, 2.828427124746190291, 14.62500000000000888 ) ) ;
#13436 = CARTESIAN_POINT ( 'NONE',  ( -10.00000000000000000, 0.000000000000000000, 0.000000000000000000 ) ) ;
#13437 = ORIENTED_EDGE ( 'NONE', *, *, #3228, .T. ) ;
#13438 = DIRECTION ( 'NONE',  ( -1.000000000000000000, 0.000000000000000000, 1.224646799147353207E-16 ) ) ;
#13439 = CARTESIAN_POINT ( 'NONE',  ( 9.920644283265380691E-16, 4.000000000000000000, 17.87500000273119483 ) ) ;
#13440 = CARTESIAN_POINT ( 'NONE',  ( 69.35000000109246798, 8.538419263543524096, 13.53841926354352054 ) ) ;
#13441 = ORIENTED_EDGE ( 'NONE', *, *, #5565, .F. ) ;
#13442 = AXIS2_PLACEMENT_3D ( 'NONE', #15779, #10509, #12416 ) ;
#13443 = CARTESIAN_POINT ( 'NONE',  ( 6.500000000000000000, 3.752776749732573247, -0.5805565836007695601 ) ) ;
#13444 = LINE ( 'NONE', #22859, #8020 ) ;
#13445 = CARTESIAN_POINT ( 'NONE',  ( 71.05000000109245661, 9.999999999999998224, 12.93301269999999192 ) ) ;
#13446 = CARTESIAN_POINT ( 'NONE',  ( -1.432654583217638944, 3.458734125000000326, 14.25000000136560629 ) ) ;
#13447 = CARTESIAN_POINT ( 'NONE',  ( 118.3095189484530181, 15.00000000000003375, 34.11836509645780069 ) ) ;
#13448 = DIRECTION ( 'NONE',  ( 1.000000000000000000, 7.703719777548943412E-32, 0.000000000000000000 ) ) ;
#13449 = CARTESIAN_POINT ( 'NONE',  ( 1.656854249492383024, -3.999999999999999112, -0.3874999999999967915 ) ) ;
#13450 = CARTESIAN_POINT ( 'NONE',  ( 0.000000000000000000, 0.000000000000000000, 0.000000000000000000 ) ) ;
#13451 = CARTESIAN_POINT ( 'NONE',  ( 44.71007725323381976, -9.000000000000000000, 5.000000000000079936 ) ) ;
#13452 = CARTESIAN_POINT ( 'NONE',  ( 4.000000000000000000, 1.656854249492381248, -1.137499999999997513 ) ) ;
#13453 = ORIENTED_EDGE ( 'NONE', *, *, #1294, .F. ) ;
#13454 = ADVANCED_FACE ( 'NONE', ( #529 ), #2794, .T. ) ;
#13455 = CARTESIAN_POINT ( 'NONE',  ( -66.85000000109248219, 9.999999999999998224, 12.93301269999999192 ) ) ;
#13456 = ORIENTED_EDGE ( 'NONE', *, *, #1502, .T. ) ;
#13457 = CARTESIAN_POINT ( 'NONE',  ( 55.68750000000000000, 9.999999999999978684, 10.99999999999999645 ) ) ;
#13458 = CARTESIAN_POINT ( 'NONE',  ( -67.30000000109247082, 12.06698730000000275, 15.85617417291294196 ) ) ;
#13459 = PRODUCT_CONTEXT ( 'NONE', #1177, 'mechanical' ) ;
#13460 = ORIENTED_EDGE ( 'NONE', *, *, #1455, .T. ) ;
#13461 = DIRECTION ( 'NONE',  ( -0.9021819276639965191, 5.282584191382421768E-17, -0.4313557341643617371 ) ) ;
#13462 = EDGE_LOOP ( 'NONE', ( #4293, #13625 ) ) ;
#13463 = VECTOR ( 'NONE', #17099, 1000.000000000000000 ) ;
#13464 = ORIENTED_EDGE ( 'NONE', *, *, #13604, .F. ) ;
#13465 = CARTESIAN_POINT ( 'NONE',  ( -3.458734124999999437, 1.432654583217640498, 15.62500000136560629 ) ) ;
#13466 = ADVANCED_FACE ( 'NONE', ( #8924 ), #1110, .T. ) ;
#13467 = CARTESIAN_POINT ( 'NONE',  ( 56.25000000000000711, 7.878679656440361612, 17.12132034355964549 ) ) ;
#13468 = CARTESIAN_POINT ( 'NONE',  ( -66.30000000109247082, 12.06698730000000275, 15.85617417291294196 ) ) ;
#13469 = CARTESIAN_POINT ( 'NONE',  ( 69.55000000109247082, 11.46158073645647235, 16.46158073645647235 ) ) ;
#13470 = CARTESIAN_POINT ( 'NONE',  ( -72.35000000000000853, 12.50000000000000000, 16.03553390593273420 ) ) ;
#13471 = DIRECTION ( 'NONE',  ( 0.000000000000000000, 0.000000000000000000, -1.000000000000000000 ) ) ;
#13472 = CARTESIAN_POINT ( 'NONE',  ( 53.96643183416157541, 7.028187705514638672, 13.68930817193508531 ) ) ;
#13473 = DIRECTION ( 'NONE',  ( 0.000000000000000000, 0.000000000000000000, 1.000000000000000000 ) ) ;
#13474 = CARTESIAN_POINT ( 'NONE',  ( 3.458734125000000770, 4.235727675282972223E-16, 5.487500001365596347 ) ) ;
#13475 = DIRECTION ( 'NONE',  ( -0.3420201433256622181, 0.9396926207859106484, 1.232595164407828100E-31 ) ) ;
#13476 = CARTESIAN_POINT ( 'NONE',  ( 4.000000000000000888, 4.898587196589412829E-16, 10.62500000273119660 ) ) ;
#13477 = CARTESIAN_POINT ( 'NONE',  ( -19.99999999999999645, -9.000000000000003553, 10.00000000000008882 ) ) ;
#13478 = ORIENTED_EDGE ( 'NONE', *, *, #20892, .T. ) ;
#13479 = ADVANCED_FACE ( 'NONE', ( #6644 ), #5629, .F. ) ;
#13480 = DIRECTION ( 'NONE',  ( 1.000000000000000000, 0.000000000000000000, 0.000000000000000000 ) ) ;
#13481 = VERTEX_POINT ( 'NONE', #12527 ) ;
#13482 = CARTESIAN_POINT ( 'NONE',  ( 59.68518183416157541, 10.06805114094562548, 11.99999999999999645 ) ) ;
#13483 = CARTESIAN_POINT ( 'NONE',  ( -3.458734125000000326, 0.000000000000000000, 2.737500001365597235 ) ) ;
#13484 = EDGE_CURVE ( 'NONE', #4626, #1632, #17373, .T. ) ;
#13485 = CARTESIAN_POINT ( 'NONE',  ( -3.458734125000000326, 0.000000000000000000, -0.2624999986344037084 ) ) ;
#13486 = VERTEX_POINT ( 'NONE', #10252 ) ;
#13487 = CARTESIAN_POINT ( 'NONE',  ( 4.000000000000000888, 4.898587196589412829E-16, 12.50000000000001066 ) ) ;
#13488 = DIRECTION ( 'NONE',  ( 1.000000000000000000, 0.000000000000000000, 0.000000000000000000 ) ) ;
#13489 = CARTESIAN_POINT ( 'NONE',  ( 23.26995556824705602, 6.748975864862779339, 10.00000000000008882 ) ) ;
#13490 = ORIENTED_EDGE ( 'NONE', *, *, #15548, .F. ) ;
#13491 = ADVANCED_FACE ( 'NONE', ( #19667 ), #8563, .F. ) ;
#13492 = EDGE_CURVE ( 'NONE', #17728, #19630, #5069, .T. ) ;
#13493 = CARTESIAN_POINT ( 'NONE',  ( -71.05000000218495870, 8.964466094067258695, 17.50000000000000355 ) ) ;
#13494 = CARTESIAN_POINT ( 'NONE',  ( -69.00000000218494733, 9.999999999999998224, 12.49999999999999289 ) ) ;
#13495 = CARTESIAN_POINT ( 'NONE',  ( 1.971781867644420635E-15, -4.000000000000000000, 15.25000000000001066 ) ) ;
#13496 = CARTESIAN_POINT ( 'NONE',  ( -2.445694354108819191, 2.445694354108820523, 19.56250000136560629 ) ) ;
#13497 = DIRECTION ( 'NONE',  ( 0.000000000000000000, 0.000000000000000000, -1.000000000000000000 ) ) ;
#13498 = CARTESIAN_POINT ( 'NONE',  ( 71.25000000109248788, 9.999999999999998224, 17.06698730000000097 ) ) ;
#13499 = CARTESIAN_POINT ( 'NONE',  ( -1.600000000000004086, 0.000000000000000000, -6.735000000000022524 ) ) ;
#13500 = CARTESIAN_POINT ( 'NONE',  ( 55.43981816583843170, 10.06805114094563791, 17.99999999999999645 ) ) ;
#13501 = CARTESIAN_POINT ( 'NONE',  ( 1.432654583217640276, 3.458734125000000770, 4.675000001365594571 ) ) ;
#13502 = CARTESIAN_POINT ( 'NONE',  ( 2.445694354108822299, -2.445694354108820079, 11.06250000136560452 ) ) ;
#13503 = AXIS2_PLACEMENT_3D ( 'NONE', #19595, #8854, #19832 ) ;
#13504 = CARTESIAN_POINT ( 'NONE',  ( -70.70000000109247651, 9.143825827087049163, 17.06698730000000097 ) ) ;
#13505 = CARTESIAN_POINT ( 'NONE',  ( -4.000000000000000000, 0.000000000000000000, -1.699999999999998401 ) ) ;
#13506 = ORIENTED_EDGE ( 'NONE', *, *, #2371, .T. ) ;
#13507 = CARTESIAN_POINT ( 'NONE',  ( 3.999999999999999112, -0.3979232138631231819, -5.929230630780099908E-17 ) ) ;
#13508 = CARTESIAN_POINT ( 'NONE',  ( -2.449293598294706907E-16, 4.000000000000000000, 5.175000002731187543 ) ) ;
#13509 = EDGE_CURVE ( 'NONE', #15051, #15217, #1225, .T. ) ;
#13510 = CARTESIAN_POINT ( 'NONE',  ( -70.05000000109247082, 9.999999999999998224, 12.93301269999999192 ) ) ;
#13511 = ORIENTED_EDGE ( 'NONE', *, *, #18009, .T. ) ;
#13512 = VERTEX_POINT ( 'NONE', #17886 ) ;
#13513 = CARTESIAN_POINT ( 'NONE',  ( 41.56848460323381289, -9.000000000000003553, 5.000000000000079936 ) ) ;
#13514 = DIRECTION ( 'NONE',  ( 0.000000000000000000, 0.000000000000000000, -1.000000000000000000 ) ) ;
#13515 = ORIENTED_EDGE ( 'NONE', *, *, #5529, .F. ) ;
#13516 = CARTESIAN_POINT ( 'NONE',  ( -1.799999999999996048, 0.000000000000000000, 0.000000000000000000 ) ) ;
#13517 = EDGE_CURVE ( 'NONE', #19575, #13757, #6876, .T. ) ;
#13518 = CARTESIAN_POINT ( 'NONE',  ( 69.00000000109247367, 7.933012699999995476, 15.85617417291294196 ) ) ;
#13519 = CARTESIAN_POINT ( 'NONE',  ( 67.65000000109247935, 7.933012699999995476, 14.99999999999999645 ) ) ;
#13520 = ORIENTED_EDGE ( 'NONE', *, *, #5073, .F. ) ;
#13521 = DIRECTION ( 'NONE',  ( 1.000000000000000000, 0.000000000000000000, 0.000000000000000000 ) ) ;
#13522 = CARTESIAN_POINT ( 'NONE',  ( 55.12500000000000711, 12.82842712474620228, 17.82842712474617386 ) ) ;
#13523 = DIRECTION ( 'NONE',  ( 0.000000000000000000, 0.000000000000000000, 1.000000000000000000 ) ) ;
#13524 = DIRECTION ( 'NONE',  ( -1.000000000000000000, -0.000000000000000000, -0.000000000000000000 ) ) ;
#13525 = CYLINDRICAL_SURFACE ( 'NONE', #23523, 4.000000000000000888 ) ;
#13526 = DIRECTION ( 'NONE',  ( 0.3420201433256622736, -0.9396926207859106484, -1.232595164407828100E-31 ) ) ;
#13527 = ORIENTED_EDGE ( 'NONE', *, *, #18112, .F. ) ;
#13528 = DIRECTION ( 'NONE',  ( 0.000000000000000000, -0.000000000000000000, -1.000000000000000000 ) ) ;
#13529 = LINE ( 'NONE', #19006, #21617 ) ;
#13530 = CARTESIAN_POINT ( 'NONE',  ( 4.999999999999999112, 0.000000000000000000, 0.000000000000000000 ) ) ;
#13531 = ORIENTED_EDGE ( 'NONE', *, *, #17394, .F. ) ;
#13532 = AXIS2_PLACEMENT_3D ( 'NONE', #10257, #1116, #21340 ) ;
#13533 = FACE_OUTER_BOUND ( 'NONE', #2959, .T. ) ;
#13534 = CARTESIAN_POINT ( 'NONE',  ( 0.000000000000000000, 0.000000000000000000, -3.700000000000000178 ) ) ;
#13535 = DIRECTION ( 'NONE',  ( 0.000000000000000000, 0.000000000000000000, 1.000000000000000000 ) ) ;
#13536 = AXIS2_PLACEMENT_3D ( 'NONE', #22174, #5431, #18238 ) ;
#13537 = ADVANCED_FACE ( 'NONE', ( #15871 ), #7556, .T. ) ;
#13538 = DIRECTION ( 'NONE',  ( 1.000000000000000000, -0.000000000000000000, -0.000000000000000000 ) ) ;
#13539 = ORIENTED_EDGE ( 'NONE', *, *, #17706, .T. ) ;
#13540 = DIRECTION ( 'NONE',  ( 1.000000000000000000, 7.703719777548943412E-32, 0.000000000000000000 ) ) ;
#13541 = VERTEX_POINT ( 'NONE', #12162 ) ;
#13542 = CARTESIAN_POINT ( 'NONE',  ( 70.95000000109247651, 11.46158073645647235, 13.53841926354352232 ) ) ;
#13543 = CARTESIAN_POINT ( 'NONE',  ( -3.999999999999999112, 1.656854249492380804, 10.93750000000001421 ) ) ;
#13544 = DIRECTION ( 'NONE',  ( 0.000000000000000000, 0.000000000000000000, -1.000000000000000000 ) ) ;
#13545 = AXIS2_PLACEMENT_3D ( 'NONE', #10526, #4993, #2938 ) ;
#13546 = ORIENTED_EDGE ( 'NONE', *, *, #8298, .T. ) ;
#13547 = DIRECTION ( 'NONE',  ( 0.000000000000000000, 1.000000000000000000, -1.224646799147353207E-16 ) ) ;
#13548 = CARTESIAN_POINT ( 'NONE',  ( 71.00000000109247367, 9.143825827087052716, 12.93301269999999192 ) ) ;
#13549 = ORIENTED_EDGE ( 'NONE', *, *, #21288, .T. ) ;
#13550 = VECTOR ( 'NONE', #9197, 1000.000000000000000 ) ;
#13551 = CARTESIAN_POINT ( 'NONE',  ( 72.50000000000000000, 9.999999999999998224, 12.49999999999999289 ) ) ;
#13552 = CARTESIAN_POINT ( 'NONE',  ( 35.00000000000000000, 7.500000000000001776, -20.00000000000000355 ) ) ;
#13553 = CARTESIAN_POINT ( 'NONE',  ( 68.85000000109246798, 12.06698730000000097, 14.99999999999999645 ) ) ;
#13554 = CARTESIAN_POINT ( 'NONE',  ( 2.445694354108821855, -2.445694354108820079, 13.81250000136560629 ) ) ;
#13555 = CYLINDRICAL_SURFACE ( 'NONE', #8232, 4.000000000000000000 ) ;
#13556 = FACE_OUTER_BOUND ( 'NONE', #8170, .T. ) ;
#13557 = VERTEX_POINT ( 'NONE', #17542 ) ;
#13558 = CARTESIAN_POINT ( 'NONE',  ( 4.000000000000000888, -1.656854249492379694, 0.7375000000000022649 ) ) ;
#13559 = CARTESIAN_POINT ( 'NONE',  ( 4.999999999999999112, 0.000000000000000000, 8.749000000000002331 ) ) ;
#13560 = CARTESIAN_POINT ( 'NONE',  ( -3.458734124999998993, 0.000000000000000000, 11.43750000136560452 ) ) ;
#13561 = CARTESIAN_POINT ( 'NONE',  ( 4.999999999999999112, 0.000000000000000000, 0.000000000000000000 ) ) ;
#13562 = PRODUCT ( 'radial cylindrical roller bearing_iso_ISO 15 RCR - 1712 - 24,SI,NC,24', 'radial cylindrical roller bearing_iso_ISO 15 RCR - 1712 - 24,SI,NC,24', '', ( #20484 ) ) ;
#13563 = VERTEX_POINT ( 'NONE', #3389 ) ;
#13564 = CARTESIAN_POINT ( 'NONE',  ( -66.35000000109248219, 11.46158073645647235, 16.46158073645647235 ) ) ;
#13565 = EDGE_LOOP ( 'NONE', ( #4589, #184, #11389, #7143, #9273, #15186, #9035, #12859, #12758, #12720, #22450, #17265 ) ) ;
#13566 = CARTESIAN_POINT ( 'NONE',  ( -68.20000000109246230, 10.85617417291294551, 17.06698729999999742 ) ) ;
#13567 = VERTEX_POINT ( 'NONE', #23266 ) ;
#13568 = DIRECTION ( 'NONE',  ( 0.000000000000000000, 0.000000000000000000, -1.000000000000000000 ) ) ;
#13569 = ORIENTED_EDGE ( 'NONE', *, *, #19710, .T. ) ;
#13570 = ORIENTED_EDGE ( 'NONE', *, *, #18466, .F. ) ;
#13571 = CARTESIAN_POINT ( 'NONE',  ( 3.458734125000002546, -1.432654583217639610, 17.12500000136560629 ) ) ;
#13572 = CARTESIAN_POINT ( 'NONE',  ( 0.7277801532338084023, -9.000000000000003553, 5.000000000000079936 ) ) ;
#13573 = CARTESIAN_POINT ( 'NONE',  ( -69.25000000109247367, 9.999999999999998224, 12.93301269999999192 ) ) ;
#13574 = PRODUCT_DEFINITION ( 'UNKNOWN', '', #3796, #22948 ) ;
#13575 = CARTESIAN_POINT ( 'NONE',  ( 68.25000000109247367, 7.933012699999995476, 14.99999999999999645 ) ) ;
#13576 = EDGE_CURVE ( 'NONE', #15433, #6393, #18010, .T. ) ;
#13577 = AXIS2_PLACEMENT_3D ( 'NONE', #19652, #3253, #12274 ) ;
#13578 = CARTESIAN_POINT ( 'NONE',  ( -67.40000000109247935, 10.85617417291294551, 17.06698729999999742 ) ) ;
#13579 = SHAPE_REPRESENTATION ( 'Machined Body Housing', ( #7318 ), #21755 ) ;
#13580 = CYLINDRICAL_SURFACE ( 'NONE', #15709, 5.000000000000000888 ) ;
#13581 = CARTESIAN_POINT ( 'NONE',  ( 57.06018183416157541, 7.000000000000000000, 14.93194885905437097 ) ) ;
#13582 = CARTESIAN_POINT ( 'NONE',  ( 38.42689195323381313, -9.000000000000001776, 10.00000000000008882 ) ) ;
#13583 = CARTESIAN_POINT ( 'NONE',  ( 3.458734125000000770, 4.235727675282972223E-16, 2.487500001365596791 ) ) ;
#13584 = DIRECTION ( 'NONE',  ( 0.3420201433256622181, -0.9396926207859107594, 0.000000000000000000 ) ) ;
#13585 = CARTESIAN_POINT ( 'NONE',  ( 2.828427124746192067, -2.828427124746189847, 10.50000000273119660 ) ) ;
#13586 = ADVANCED_FACE ( 'NONE', ( #14197 ), #6757, .F. ) ;
#13587 = LINE ( 'NONE', #13477, #22575 ) ;
#13588 = ORIENTED_EDGE ( 'NONE', *, *, #21634, .T. ) ;
#13589 = FACE_BOUND ( 'NONE', #16238, .T. ) ;
#13590 = ORIENTED_EDGE ( 'NONE', *, *, #13812, .T. ) ;
#13591 = CARTESIAN_POINT ( 'NONE',  ( 51.00000000000000711, 12.12132034355963484, 12.87867965644034740 ) ) ;
#13592 = DIRECTION ( 'NONE',  ( 0.000000000000000000, 0.000000000000000000, 1.000000000000000000 ) ) ;
#13593 = CARTESIAN_POINT ( 'NONE',  ( -2.117863837641485618E-16, 3.458734125000000326, 3.487500001365594571 ) ) ;
#13594 = CARTESIAN_POINT ( 'NONE',  ( -4.000000000000000000, -2.309401076758515803, -0.4999999999999995559 ) ) ;
#13595 = EDGE_LOOP ( 'NONE', ( #11719, #10640, #2164, #15598, #17967, #8151, #15232, #3295, #9124, #20570, #7838, #6344, #15159, #1529, #13432, #8068, #3534, #16329, #1412 ) ) ;
#13596 = AXIS2_PLACEMENT_3D ( 'NONE', #16608, #187, #7518 ) ;
#13597 = CARTESIAN_POINT ( 'NONE',  ( -3.999999999999999112, 1.656854249492380804, 14.93750000000000888 ) ) ;
#13598 = SURFACE_STYLE_USAGE ( .BOTH. , #9890 ) ;
#13599 = AXIS2_PLACEMENT_3D ( 'NONE', #5136, #21055, #4667 ) ;
#13600 = DIRECTION ( 'NONE',  ( 0.000000000000000000, -0.000000000000000000, 1.000000000000000000 ) ) ;
#13601 = ORIENTED_EDGE ( 'NONE', *, *, #9801, .F. ) ;
#13602 = DIRECTION ( 'NONE',  ( -1.000000000000000000, -0.000000000000000000, 0.000000000000000000 ) ) ;
#13603 = CARTESIAN_POINT ( 'NONE',  ( -1.432654583217641164, -3.458734125000000326, -1.824999998634404097 ) ) ;
#13604 = EDGE_CURVE ( 'NONE', #17274, #7791, #22014, .T. ) ;
#13605 = CYLINDRICAL_SURFACE ( 'NONE', #23280, 4.000000000000000000 ) ;
#13606 = CARTESIAN_POINT ( 'NONE',  ( 66.29999999999999716, 7.499999999999996447, 14.99999999999999645 ) ) ;
#13607 = EDGE_CURVE ( 'NONE', #11847, #7761, #11782, .T. ) ;
#13608 = CARTESIAN_POINT ( 'NONE',  ( 12.68853974071656232, -8.974600000000002353, 10.00000000000008882 ) ) ;
#13609 = CARTESIAN_POINT ( 'NONE',  ( 68.10000000109246798, 9.143825827087049163, 17.06698729999999742 ) ) ;
#13611 = CARTESIAN_POINT ( 'NONE',  ( 70.85000000218494165, 12.50000000000000000, 16.03553390593273775 ) ) ;
#13610 = CIRCLE ( 'NONE', #14002, 5.000000000000000888 ) ;
#13612 = CARTESIAN_POINT ( 'NONE',  ( 53.84606816583843880, 8.825410453826357582, 18.02818770551464667 ) ) ;
#13613 = AXIS2_PLACEMENT_3D ( 'NONE', #13992, #12206, #1972 ) ;
#13614 = CARTESIAN_POINT ( 'NONE',  ( 3.458734125000000326, 1.432654583217640498, -2.699999998634404541 ) ) ;
#13615 = CARTESIAN_POINT ( 'NONE',  ( 1.432654583217643163, -3.458734124999999882, 11.00000000136560452 ) ) ;
#13616 = ADVANCED_FACE ( 'NONE', ( #17664 ), #21455, .T. ) ;
#13617 = LINE ( 'NONE', #8114, #765 ) ;
#13618 = CARTESIAN_POINT ( 'NONE',  ( -68.10000000109246798, 12.06698729999999919, 15.85617417291294196 ) ) ;
#13619 = DIRECTION ( 'NONE',  ( 0.000000000000000000, 0.000000000000000000, -1.000000000000000000 ) ) ;
#13620 = CARTESIAN_POINT ( 'NONE',  ( 4.999999999999999112, 9.314797388894893615, 1.239665997526919083 ) ) ;
#13621 = ORIENTED_EDGE ( 'NONE', *, *, #6464, .T. ) ;
#13622 = FACE_OUTER_BOUND ( 'NONE', #6854, .T. ) ;
#13623 = CARTESIAN_POINT ( 'NONE',  ( 2.828427124746190735, -2.828427124746189847, 3.800000002731186211 ) ) ;
#13624 = ORIENTED_EDGE ( 'NONE', *, *, #1236, .F. ) ;
#13625 = ORIENTED_EDGE ( 'NONE', *, *, #15236, .T. ) ;
#13626 = AXIS2_PLACEMENT_3D ( 'NONE', #11742, #19244, #20799 ) ;
#13627 = DIRECTION ( 'NONE',  ( 0.000000000000000000, 0.000000000000000000, 1.000000000000000000 ) ) ;
#13628 = CARTESIAN_POINT ( 'NONE',  ( 52.50000000000000711, 12.82842712474617741, 12.17157287525379239 ) ) ;
#13629 = ORIENTED_EDGE ( 'NONE', *, *, #7938, .T. ) ;
#13630 = CARTESIAN_POINT ( 'NONE',  ( 4.236525694536557474, -2.416953475386482530, -3.751298745799839462 ) ) ;
#13631 = EDGE_CURVE ( 'NONE', #22338, #2643, #3148, .T. ) ;
#13632 = AXIS2_PLACEMENT_3D ( 'NONE', #915, #12090, #13993 ) ;
#13633 = CARTESIAN_POINT ( 'NONE',  ( 67.90000000109246514, 12.06698730000000275, 15.85617417291294196 ) ) ;
#13634 = CARTESIAN_POINT ( 'NONE',  ( 67.95000000109247651, 11.46158073645647235, 13.53841926354352232 ) ) ;
#13635 = ADVANCED_FACE ( 'NONE', ( #11278 ), #15227, .T. ) ;
#13636 = ORIENTED_EDGE ( 'NONE', *, *, #11868, .F. ) ;
#13637 = CARTESIAN_POINT ( 'NONE',  ( -3.847601380332740018, -11.25000000000000355, 5.000000000000079936 ) ) ;
#13638 = CARTESIAN_POINT ( 'NONE',  ( 54.84375000000000000, 8.343145750507638070, 19.00000000000000711 ) ) ;
#13639 = CARTESIAN_POINT ( 'NONE',  ( -3.999999999999998224, -1.656854249492383024, 12.18750000273119838 ) ) ;
#13640 = EDGE_CURVE ( 'NONE', #16324, #8317, #11398, .T. ) ;
#13641 = DIRECTION ( 'NONE',  ( 0.000000000000000000, 0.000000000000000000, 1.000000000000000000 ) ) ;
#13642 = CARTESIAN_POINT ( 'NONE',  ( -65.00000000000000000, 9.999999999999998224, 12.49999999999999289 ) ) ;
#13643 = ADVANCED_FACE ( 'NONE', ( #11531 ), #6794, .T. ) ;
#13644 = CARTESIAN_POINT ( 'NONE',  ( 0.000000000000000000, 0.000000000000000000, -3.700000000000000178 ) ) ;
#13645 = ORIENTED_EDGE ( 'NONE', *, *, #585, .T. ) ;
#13646 = CYLINDRICAL_SURFACE ( 'NONE', #17223, 8.749000000000002331 ) ;
#13647 = CARTESIAN_POINT ( 'NONE',  ( 2.500000000000000000, 0.000000000000000000, 0.000000000000000000 ) ) ;
#13648 = FACE_OUTER_BOUND ( 'NONE', #5970, .T. ) ;
#13649 = ORIENTED_EDGE ( 'NONE', *, *, #4072, .F. ) ;
#13650 = CARTESIAN_POINT ( 'NONE',  ( 16.43574340323381122, -9.000000000000003553, 5.000000000000079936 ) ) ;
#13651 = CARTESIAN_POINT ( 'NONE',  ( 54.99999999999996447, -15.00000000000000000, 5.000000000000003553 ) ) ;
#13652 = CARTESIAN_POINT ( 'NONE',  ( 45.00000000000000000, -10.00000000000001599, 34.11836509645782201 ) ) ;
#13653 = PRODUCT_DEFINITION_CONTEXT ( 'detailed design', #3495, 'design' ) ;
#13654 = DIRECTION ( 'NONE',  ( 0.000000000000000000, -0.4999999999999989453, 0.8660254037844391517 ) ) ;
#13655 = VERTEX_POINT ( 'NONE', #16650 ) ;
#13656 = CARTESIAN_POINT ( 'NONE',  ( -2.828427124746190291, 2.828427124746190291, 1.175000000000000711 ) ) ;
#13657 = ORIENTED_EDGE ( 'NONE', *, *, #11168, .F. ) ;
#13658 = PLANE ( 'NONE',  #23650 ) ;
#13659 = DIRECTION ( 'NONE',  ( 0.3420201433256622181, -0.9396926207859107594, 0.000000000000000000 ) ) ;
#13660 = CARTESIAN_POINT ( 'NONE',  ( 69.80000000218494449, 9.999999999999998224, 12.49999999999999289 ) ) ;
#13661 = MANIFOLD_SOLID_BREP ( 'Mirror2', #14697 ) ;
#13662 = CARTESIAN_POINT ( 'NONE',  ( 14.99999999999999289, -10.00000000000000000, -50.00000000000000000 ) ) ;
#13663 = CARTESIAN_POINT ( 'NONE',  ( -2.687328764639638656, 3.067272167851286202, -0.05923475698270370959 ) ) ;
#13664 = CARTESIAN_POINT ( 'NONE',  ( 66.75000000109245946, 8.538419263543522320, 16.46158073645647235 ) ) ;
#13665 = VERTEX_POINT ( 'NONE', #587 ) ;
#13666 = CARTESIAN_POINT ( 'NONE',  ( -68.75000000218494733, 7.499999999999996447, 16.03553390593273775 ) ) ;
#13667 = EDGE_CURVE ( 'NONE', #12476, #1631, #1587, .T. ) ;
#13668 = DIRECTION ( 'NONE',  ( -1.000000000000000000, 0.000000000000000000, 0.000000000000000000 ) ) ;
#13669 = EDGE_CURVE ( 'NONE', #8446, #17296, #2139, .T. ) ;
#13670 = CARTESIAN_POINT ( 'NONE',  ( 71.35000000109246798, 11.46158073645647235, 16.46158073645647235 ) ) ;
#13671 = CARTESIAN_POINT ( 'NONE',  ( 1.432654583217643163, -3.458734124999999437, 12.75000000136560629 ) ) ;
#13672 = CARTESIAN_POINT ( 'NONE',  ( 0.000000000000000000, 0.000000000000000000, -3.699999999999998401 ) ) ;
#13673 = EDGE_CURVE ( 'NONE', #3210, #9951, #9607, .T. ) ;
#13674 = CARTESIAN_POINT ( 'NONE',  ( 34.99999999999999289, 4.500000000000001776, -50.00000000000000000 ) ) ;
#13675 = ORIENTED_EDGE ( 'NONE', *, *, #20801, .T. ) ;
#13676 = CARTESIAN_POINT ( 'NONE',  ( 1.656854249492380360, 4.000000000000000000, -0.01249999999999832322 ) ) ;
#13677 = DIRECTION ( 'NONE',  ( 0.000000000000000000, 0.000000000000000000, 1.000000000000000000 ) ) ;
#13678 = CARTESIAN_POINT ( 'NONE',  ( 0.7277801532338118440, -9.000000000000003553, 10.00000000000008882 ) ) ;
#13679 = CARTESIAN_POINT ( 'NONE',  ( 4.999999999999999112, 0.000000000000000000, 0.000000000000000000 ) ) ;
#13680 = ORIENTED_EDGE ( 'NONE', *, *, #14033, .F. ) ;
#13681 = CARTESIAN_POINT ( 'NONE',  ( -65.70000000109247651, 9.143825827087049163, 17.06698730000000097 ) ) ;
#13682 = ORIENTED_EDGE ( 'NONE', *, *, #13943, .T. ) ;
#13683 = VECTOR ( 'NONE', #16112, 1000.000000000000000 ) ;
#13684 = CARTESIAN_POINT ( 'NONE',  ( -69.25000000109245946, 7.933012699999995476, 14.99999999999999645 ) ) ;
#13685 = ORIENTED_EDGE ( 'NONE', *, *, #15382, .F. ) ;
#13686 = CARTESIAN_POINT ( 'NONE',  ( -2.449293598294706907E-16, 4.000000000000000000, -1.824999997268811791 ) ) ;
#13687 = ORIENTED_EDGE ( 'NONE', *, *, #17482, .F. ) ;
#13688 = AXIS2_PLACEMENT_3D ( 'NONE', #20643, #878, #18851 ) ;
#13689 = ORIENTED_EDGE ( 'NONE', *, *, #6969, .F. ) ;
#13690 = CARTESIAN_POINT ( 'NONE',  ( 1.432654583217643163, -3.458734124999999882, 12.00000000136560452 ) ) ;
#13691 = CARTESIAN_POINT ( 'NONE',  ( 65.00000000000000000, 15.00000000000000000, 19.99999999999999645 ) ) ;
#13692 = VECTOR ( 'NONE', #19228, 1000.000000000000000 ) ;
#13693 = VECTOR ( 'NONE', #22735, 1000.000000000000000 ) ;
#13694 = CARTESIAN_POINT ( 'NONE',  ( 22.70968385928345157, -8.974600000000002353, 5.000000000000079936 ) ) ;
#13695 = CARTESIAN_POINT ( 'NONE',  ( 66.95000000109246230, 11.46158073645647235, 13.53841926354352232 ) ) ;
#13696 = CARTESIAN_POINT ( 'NONE',  ( -68.10000000109245377, 12.06698730000000275, 15.85617417291294196 ) ) ;
#13697 = CARTESIAN_POINT ( 'NONE',  ( 11.86036186966726191, -11.25000000000000355, 10.00000000000008882 ) ) ;
#13698 = CARTESIAN_POINT ( 'NONE',  ( 58.84143183416158962, 8.689308171935088865, 17.97181229448535689 ) ) ;
#13699 = LINE ( 'NONE', #9750, #14288 ) ;
#13700 = AXIS2_PLACEMENT_3D ( 'NONE', #6531, #17314, #8106 ) ;
#13701 = CARTESIAN_POINT ( 'NONE',  ( 1.432654583217640276, 3.458734125000000770, 3.675000001365597235 ) ) ;
#13702 = CARTESIAN_POINT ( 'NONE',  ( 71.34999999999999432, 11.03553390593268269, 12.49999999999994138 ) ) ;
#13703 = CARTESIAN_POINT ( 'NONE',  ( -3.999999999999998224, -1.656854249492383246, 10.18750000273119660 ) ) ;
#13704 = PLANE ( 'NONE',  #12283 ) ;
#13705 = AXIS2_PLACEMENT_3D ( 'NONE', #19931, #19689, #1366 ) ;
#13706 = CIRCLE ( 'NONE', #21689, 2.649999999999999467 ) ;
#13707 = ORIENTED_EDGE ( 'NONE', *, *, #3069, .F. ) ;
#13708 = CARTESIAN_POINT ( 'NONE',  ( -3.999999999999999112, 0.000000000000000000, 17.12500000273119838 ) ) ;
#13709 = EDGE_LOOP ( 'NONE', ( #6038, #12192, #22754, #3780, #22789 ) ) ;
#13710 = CARTESIAN_POINT ( 'NONE',  ( 51.09375000000000000, 11.24264068711927322, 11.99999999999998934 ) ) ;
#13711 = CARTESIAN_POINT ( 'NONE',  ( -1.432654583217640942, -3.458734124999999882, 0.9250000013655964581 ) ) ;
#13712 = CARTESIAN_POINT ( 'NONE',  ( 3.458734125000000326, 1.432654583217640498, 0.3000000013655960140 ) ) ;
#13713 = ORIENTED_EDGE ( 'NONE', *, *, #14798, .T. ) ;
#13714 = DIRECTION ( 'NONE',  ( -1.000000000000000000, 0.000000000000000000, 0.000000000000000000 ) ) ;
#13715 = ADVANCED_FACE ( 'NONE', ( #16899 ), #353, .F. ) ;
#13716 = DIRECTION ( 'NONE',  ( -0.000000000000000000, -0.000000000000000000, 1.000000000000000000 ) ) ;
#13717 = EDGE_LOOP ( 'NONE', ( #16891, #21203, #7822, #22740 ) ) ;
#13718 = DIRECTION ( 'NONE',  ( 0.000000000000000000, -0.5877852522924801315, 0.8090169943749423442 ) ) ;
#13719 = ORIENTED_EDGE ( 'NONE', *, *, #23438, .T. ) ;
#13720 = CARTESIAN_POINT ( 'NONE',  ( 54.87731816583843170, 7.830560233210212218, 12.92679907967049679 ) ) ;
#13721 = CARTESIAN_POINT ( 'NONE',  ( -71.25000000218494733, 7.499999999999995559, 13.96446609406725692 ) ) ;
#13722 =( BOUNDED_CURVE ( )  B_SPLINE_CURVE ( 2, ( #5621, #21041, #13656, #11637, #9600, #15222, #8150, #19143, #22487 ),
 .UNSPECIFIED., .F., .F. ) 
 B_SPLINE_CURVE_WITH_KNOTS ( ( 3, 2, 2, 2, 3 ),
 ( 0.5000000000000000000, 0.5124999999999999556, 0.5250000000000000222, 0.5374999999999999778, 0.5500000000000000444 ),
 .UNSPECIFIED. ) 
 CURVE ( )  GEOMETRIC_REPRESENTATION_ITEM ( )  RATIONAL_B_SPLINE_CURVE ( ( 1.000000000000000000, 0.9238795325112867385, 1.000000000000000000, 0.9238795325112867385, 1.000000000000000000, 0.9238795325112867385, 1.000000000000000000, 0.9238795325112867385, 1.000000000000000000 ) ) 
 REPRESENTATION_ITEM ( '' )  );
#13723 = DIRECTION ( 'NONE',  ( -7.087422195345011518E-32, -1.000000000000000000, -0.000000000000000000 ) ) ;
#13724 = VECTOR ( 'NONE', #1134, 1000.000000000000000 ) ;
#13725 = CARTESIAN_POINT ( 'NONE',  ( 4.999999999999999112, 8.475820894093034852, -4.057423117305300586 ) ) ;
#13726 =( GEOMETRIC_REPRESENTATION_CONTEXT ( 3 ) GLOBAL_UNCERTAINTY_ASSIGNED_CONTEXT ( ( #13159 ) ) GLOBAL_UNIT_ASSIGNED_CONTEXT ( ( #21322, #2781, #759 ) ) REPRESENTATION_CONTEXT ( 'NONE', 'WORKASPACE' ) );
#13727 = CARTESIAN_POINT ( 'NONE',  ( 2.445694354108821411, 2.445694354108820523, 19.31250000136560629 ) ) ;
#13728 = LINE ( 'NONE', #9775, #9341 ) ;
#13729 = CARTESIAN_POINT ( 'NONE',  ( 70.15000000109247935, 11.46158073645647235, 13.53841926354352232 ) ) ;
#13730 = CARTESIAN_POINT ( 'NONE',  ( 4.999999999999999112, 4.472189673936902921, -8.264486777890061475 ) ) ;
#13731 = CARTESIAN_POINT ( 'NONE',  ( 54.50231816583843170, 12.07320092032949610, 12.83056023321021044 ) ) ;
#13732 = CARTESIAN_POINT ( 'NONE',  ( 3.458734125000000770, 1.432654583217640498, 0.5500000013655963471 ) ) ;
#13733 = CARTESIAN_POINT ( 'NONE',  ( -1.432654583217639166, 3.458734125000000770, 11.50000000136560629 ) ) ;
#13734 = CARTESIAN_POINT ( 'NONE',  ( -67.85000000109246798, 9.999999999999998224, 12.93301269999999192 ) ) ;
#13735 = AXIS2_PLACEMENT_3D ( 'NONE', #3149, #17665, #19318 ) ;
#13736 = DIRECTION ( 'NONE',  ( 1.000000000000000000, 0.000000000000000000, 0.000000000000000000 ) ) ;
#13737 = DIRECTION ( 'NONE',  ( 0.000000000000000000, -0.3090169943749350168, -0.9510565162951576390 ) ) ;
#13738 = VERTEX_POINT ( 'NONE', #15116 ) ;
#13739 = CARTESIAN_POINT ( 'NONE',  ( -2.807080416178626692, 3.225969019225154444, -3.502507215260441065 ) ) ;
#13740 = FILL_AREA_STYLE ('',( #12070 ) ) ;
#13741 = CARTESIAN_POINT ( 'NONE',  ( -1.656854249492381248, -3.999999999999999112, 2.612500002731188431 ) ) ;
#13742 = ORIENTED_EDGE ( 'NONE', *, *, #5031, .T. ) ;
#13743 = ORIENTED_EDGE ( 'NONE', *, *, #7439, .F. ) ;
#13744 = ADVANCED_FACE ( 'NONE', ( #5986 ), #20582, .F. ) ;
#13745 = CARTESIAN_POINT ( 'NONE',  ( -4.000000000000000000, -1.656854249492383024, 1.487500002731187321 ) ) ;
#13746 = VECTOR ( 'NONE', #7524, 1000.000000000000000 ) ;
#13747 = EDGE_CURVE ( 'NONE', #18227, #22338, #6427, .T. ) ;
#13748 = DIRECTION ( 'NONE',  ( -0.3420201433256622181, 0.9396926207859106484, 1.232595164407828100E-31 ) ) ;
#13749 = VERTEX_POINT ( 'NONE', #17127 ) ;
#13750 = FACE_BOUND ( 'NONE', #19204, .T. ) ;
#13751 = VECTOR ( 'NONE', #19375, 1000.000000000000000 ) ;
#13752 = EDGE_CURVE ( 'NONE', #20363, #20481, #4120, .T. ) ;
#13753 = CARTESIAN_POINT ( 'NONE',  ( 66.95000000109246230, 11.46158073645647235, 13.53841926354352232 ) ) ;
#13754 = CIRCLE ( 'NONE', #12240, 9.999999999999996447 ) ;
#13755 = CARTESIAN_POINT ( 'NONE',  ( 68.65000000109246514, 9.999999999999998224, 12.93301269999999192 ) ) ;
#13756 = PRODUCT ( 'End Stop Bumper spring', 'End Stop Bumper spring', '', ( #13459 ) ) ;
#13757 = VERTEX_POINT ( 'NONE', #934 ) ;
#13758 = PRODUCT_DEFINITION_FORMATION_WITH_SPECIFIED_SOURCE ( 'ANY', '', #13756, .NOT_KNOWN. ) ;
#13759 =( BOUNDED_CURVE ( )  B_SPLINE_CURVE ( 2, ( #18022, #1598, #400, #43, #16694, #13003, #16464, #11206, #13123 ),
 .UNSPECIFIED., .F., .F. ) 
 B_SPLINE_CURVE_WITH_KNOTS ( ( 3, 2, 2, 2, 3 ),
 ( 0.3125000000000002776, 0.3281250000000001665, 0.3437500000000001110, 0.3593750000000000000, 0.3749999999999998890 ),
 .UNSPECIFIED. ) 
 CURVE ( )  GEOMETRIC_REPRESENTATION_ITEM ( )  RATIONAL_B_SPLINE_CURVE ( ( 0.9999999999999986677, 0.9238795325112880708, 1.000000000000000000, 0.9238795325112867385, 1.000000000000000000, 0.9238795325112867385, 1.000000000000000000, 0.9238795325112872936, 0.9999999999999994449 ) ) 
 REPRESENTATION_ITEM ( '' )  );
#13760 = CARTESIAN_POINT ( 'NONE',  ( 65.00000000000000000, -10.00000000000000178, 17.49999999999999645 ) ) ;
#13761 = CIRCLE ( 'NONE', #6102, 2.041999999999999815 ) ;
#13762 = CARTESIAN_POINT ( 'NONE',  ( 56.81250000000000000, 14.00000000000000000, 14.99999999999997691 ) ) ;
#13763 = DIRECTION ( 'NONE',  ( 1.000000000000000000, 0.000000000000000000, -0.000000000000000000 ) ) ;
#13764 = CARTESIAN_POINT ( 'NONE',  ( -8.696997796766188671, -9.000000000000003553, 5.000000000000079936 ) ) ;
#13765 = DIRECTION ( 'NONE',  ( 0.000000000000000000, 0.000000000000000000, -1.000000000000000000 ) ) ;
#13766 =( REPRESENTATION_RELATIONSHIP ('NONE','NONE', #8403, #15757 ) REPRESENTATION_RELATIONSHIP_WITH_TRANSFORMATION ( #21068 )SHAPE_REPRESENTATION_RELATIONSHIP( ) );
#13767 = CARTESIAN_POINT ( 'NONE',  ( -2.423057340716551433, -8.974600000000002353, 5.000000000000079936 ) ) ;
#13768 = EDGE_LOOP ( 'NONE', ( #2988, #12083, #11044, #767 ) ) ;
#13769 = CARTESIAN_POINT ( 'NONE',  ( 4.999999999999999112, 0.000000000000000000, 0.000000000000000000 ) ) ;
#13770 = DIRECTION ( 'NONE',  ( 1.000000000000000000, 0.000000000000000000, 0.000000000000000000 ) ) ;
#13771 = CARTESIAN_POINT ( 'NONE',  ( 0.000000000000000000, 8.152713396088763886, 3.174628368996105010 ) ) ;
#13772 = AXIS2_PLACEMENT_3D ( 'NONE', #11530, #5985, #5868 ) ;
#13773 = EDGE_LOOP ( 'NONE', ( #12806, #7927, #13971, #3023 ) ) ;
#13774 = VECTOR ( 'NONE', #14979, 1000.000000000000000 ) ;
#13775 = FACE_OUTER_BOUND ( 'NONE', #1687, .T. ) ;
#13776 = EDGE_CURVE ( 'NONE', #16324, #20947, #7576, .T. ) ;
#13777 = DIRECTION ( 'NONE',  ( 0.000000000000000000, 0.000000000000000000, -1.000000000000000000 ) ) ;
#13778 = DIRECTION ( 'NONE',  ( 1.000000000000000000, -0.000000000000000000, -0.000000000000000000 ) ) ;
#13779 = EDGE_CURVE ( 'NONE', #7617, #22160, #20923, .T. ) ;
#13780 = CARTESIAN_POINT ( 'NONE',  ( 19.99999999999999645, 4.500000000000003553, -50.00000000000000000 ) ) ;
#13781 = ORIENTED_EDGE ( 'NONE', *, *, #11696, .T. ) ;
#13782 = CARTESIAN_POINT ( 'NONE',  ( 1.067197363239223762, 6.889406814520512512, -0.2573354458087852570 ) ) ;
#13783 = EDGE_LOOP ( 'NONE', ( #8442, #2777, #9678, #4348 ) ) ;
#13784 = CARTESIAN_POINT ( 'NONE',  ( 71.35000000109246798, 8.538419263543522320, 16.46158073645647235 ) ) ;
#13785 = PRESENTATION_LAYER_ASSIGNMENT (  '', '', ( #6504 ) ) ;
#13786 = EDGE_CURVE ( 'NONE', #15640, #9577, #19789, .T. ) ;
#13787 = CARTESIAN_POINT ( 'NONE',  ( 70.90000000218495302, 11.76776695296636888, 16.76776695296636532 ) ) ;
#13788 = EDGE_CURVE ( 'NONE', #19958, #23289, #4759, .T. ) ;
#13789 = DIRECTION ( 'NONE',  ( 1.000000000000000000, 7.703719777548943412E-32, 0.000000000000000000 ) ) ;
#13790 = CARTESIAN_POINT ( 'NONE',  ( 0.2500000000000002220, 0.000000000000000000, 0.000000000000000000 ) ) ;
#13791 = CARTESIAN_POINT ( 'NONE',  ( 68.05000000109247082, 12.06698730000000097, 14.99999999999999645 ) ) ;
#13792 = ORIENTED_EDGE ( 'NONE', *, *, #21493, .F. ) ;
#13793 = VECTOR ( 'NONE', #2303, 1000.000000000000000 ) ;
#13794 = VECTOR ( 'NONE', #21372, 1000.000000000000114 ) ;
#13795 = DIRECTION ( 'NONE',  ( 0.000000000000000000, 0.000000000000000000, -1.000000000000000000 ) ) ;
#13796 = CARTESIAN_POINT ( 'NONE',  ( 68.70000000109246230, 10.85617417291294551, 12.93301269999999370 ) ) ;
#13797 = CARTESIAN_POINT ( 'NONE',  ( -3.458734124999998993, -1.432654583217642497, 12.50000000136560452 ) ) ;
#13798 = AXIS2_PLACEMENT_3D ( 'NONE', #2120, #9454, #22354 ) ;
#13799 = FACE_OUTER_BOUND ( 'NONE', #11779, .T. ) ;
#13800 = CARTESIAN_POINT ( 'NONE',  ( 0.000000000000000000, 0.000000000000000000, 0.000000000000000000 ) ) ;
#13801 = AXIS2_PLACEMENT_3D ( 'NONE', #1093, #21200, #8547 ) ;
#13802 = ORIENTED_EDGE ( 'NONE', *, *, #2597, .F. ) ;
#13803 = CARTESIAN_POINT ( 'NONE',  ( -1.857128706618043301, 2.924396244061969519, -3.295601554149324208 ) ) ;
#13804 = LINE ( 'NONE', #19162, #5961 ) ;
#13805 = LINE ( 'NONE', #15723, #7013 ) ;
#13806 = DIRECTION ( 'NONE',  ( 0.000000000000000000, 0.000000000000000000, 1.000000000000000000 ) ) ;
#13807 = VERTEX_POINT ( 'NONE', #13900 ) ;
#13808 = LINE ( 'NONE', #4321, #944 ) ;
#13809 = EDGE_LOOP ( 'NONE', ( #12038, #380, #86, #16880 ) ) ;
#13810 = CARTESIAN_POINT ( 'NONE',  ( -69.05000000109247082, 9.999999999999998224, 17.06698730000000097 ) ) ;
#13811 = CONTEXT_DEPENDENT_SHAPE_REPRESENTATION ( #13766, #15089 ) ;
#13812 = EDGE_CURVE ( 'NONE', #16753, #23445, #9489, .T. ) ;
#13813 = ORIENTED_EDGE ( 'NONE', *, *, #241, .F. ) ;
#13814 = ORIENTED_EDGE ( 'NONE', *, *, #10842, .T. ) ;
#13815 = EDGE_CURVE ( 'NONE', #5142, #19833, #8389, .T. ) ;
#13816 = ORIENTED_EDGE ( 'NONE', *, *, #7894, .T. ) ;
#13817 = CARTESIAN_POINT ( 'NONE',  ( -3.458734124999999437, 0.000000000000000000, 12.68750000136560629 ) ) ;
#13818 = CARTESIAN_POINT ( 'NONE',  ( 51.56250000000000711, 6.999999999999997335, 15.00000000000000533 ) ) ;
#13819 = VECTOR ( 'NONE', #11166, 1000.000000000000000 ) ;
#13820 = EDGE_CURVE ( 'NONE', #11553, #4495, #19028, .T. ) ;
#13821 = CARTESIAN_POINT ( 'NONE',  ( 4.999999999999999112, -7.360373001730883935, -4.729683950898952105 ) ) ;
#13822 = COLOUR_RGB ( '', 0.66274510, 0.83137255, 0.94901961) ;
#13823 = CARTESIAN_POINT ( 'NONE',  ( 66.90000000109247935, 10.85617417291294551, 12.93301269999999192 ) ) ;
#13824 = CARTESIAN_POINT ( 'NONE',  ( -70.25000000000000000, 7.499999999999995559, 16.03553390593273420 ) ) ;
#13825 = DIRECTION ( 'NONE',  ( 0.3420201433256622181, -0.9396926207859107594, 0.000000000000000000 ) ) ;
#13826 = CARTESIAN_POINT ( 'NONE',  ( 57.99768183416157541, 12.87654654797631792, 12.21969229848393113 ) ) ;
#13827 = DIRECTION ( 'NONE',  ( 1.000000000000000000, 0.000000000000000000, -1.224646799147353207E-16 ) ) ;
#13828 = CARTESIAN_POINT ( 'NONE',  ( -3.458734125000000770, 0.000000000000000000, -1.012499998634402543 ) ) ;
#13829 = DIRECTION ( 'NONE',  ( 0.000000000000000000, 0.000000000000000000, 1.000000000000000000 ) ) ;
#13830 = CARTESIAN_POINT ( 'NONE',  ( 10.14331325928345073, -8.974600000000002353, 5.000000000000079936 ) ) ;
#13831 = CARTESIAN_POINT ( 'NONE',  ( -3.999999999999999112, 0.000000000000000000, 13.12500000273119660 ) ) ;
#13832 = LINE ( 'NONE', #16321, #3450 ) ;
#13833 = CIRCLE ( 'NONE', #15749, 11.00000000000000000 ) ;
#13834 = ORIENTED_EDGE ( 'NONE', *, *, #23599, .T. ) ;
#13835 = CARTESIAN_POINT ( 'NONE',  ( 14.99999999999999289, -10.00000000000000000, -50.00000000000000000 ) ) ;
#13836 = ORIENTED_EDGE ( 'NONE', *, *, #8605, .T. ) ;
#13837 = CARTESIAN_POINT ( 'NONE',  ( 59.02893183416158251, 11.58880310854676132, 19.02818770551463956 ) ) ;
#13838 = PRESENTATION_STYLE_ASSIGNMENT (( #15634 ) ) ;
#13839 = CARTESIAN_POINT ( 'NONE',  ( 3.458734125000000326, 4.235727675282971730E-16, -0.7624999986344040970 ) ) ;
#13840 = VERTEX_POINT ( 'NONE', #8157 ) ;
#13841 = CYLINDRICAL_SURFACE ( 'NONE', #14878, 8.265000000000021885 ) ;
#13842 = EDGE_LOOP ( 'NONE', ( #6245, #2872, #4817, #2976 ) ) ;
#13843 = CARTESIAN_POINT ( 'NONE',  ( 4.999999999999999112, -8.461683424509331530, 2.223716399045538861 ) ) ;
#13844 = EDGE_LOOP ( 'NONE', ( #1750, #18693 ) ) ;
#13845 = EDGE_CURVE ( 'NONE', #21424, #21411, #10524, .T. ) ;
#13846 = CARTESIAN_POINT ( 'NONE',  ( 55.43981816583843170, 10.06805114094563791, 17.99999999999999645 ) ) ;
#13847 = CARTESIAN_POINT ( 'NONE',  ( -66.60000000218495586, 9.999999999999998224, 12.49999999999999289 ) ) ;
#13848 = DIRECTION ( 'NONE',  ( 1.224646799147353207E-16, -0.000000000000000000, 1.000000000000000000 ) ) ;
#13849 = CARTESIAN_POINT ( 'NONE',  ( -71.85000000109246798, 9.999999999999998224, 12.93301269999999192 ) ) ;
#13850 = CARTESIAN_POINT ( 'NONE',  ( 66.34999999999999432, 7.499999999999995559, 13.96446609406725692 ) ) ;
#13851 = CARTESIAN_POINT ( 'NONE',  ( 9.920644283265380691E-16, 4.000000000000000000, 14.87500000273119660 ) ) ;
#13852 = DIRECTION ( 'NONE',  ( 0.000000000000000000, 0.000000000000000000, 1.000000000000000000 ) ) ;
#13853 = CARTESIAN_POINT ( 'NONE',  ( 69.40000000109249356, 12.06698730000000275, 14.14382582708705094 ) ) ;
#13854 = PLANE ( 'NONE',  #3061 ) ;
#13855 = CARTESIAN_POINT ( 'NONE',  ( 57.40856816583844591, 12.97181229448534978, 13.68930817193506755 ) ) ;
#13856 = CARTESIAN_POINT ( 'NONE',  ( 3.458734125000001214, -1.432654583217639610, 3.425000001365596791 ) ) ;
#13857 = CARTESIAN_POINT ( 'NONE',  ( 67.80000000218494449, 9.999999999999998224, 17.49999999999999645 ) ) ;
#13858 = DIRECTION ( 'NONE',  ( 0.000000000000000000, 0.000000000000000000, 1.000000000000000000 ) ) ;
#13859 = CARTESIAN_POINT ( 'NONE',  ( -69.00000000109245946, 10.85617417291294551, 17.06698730000000097 ) ) ;
#13860 = ORIENTED_EDGE ( 'NONE', *, *, #23533, .T. ) ;
#13861 = DIRECTION ( 'NONE',  ( 0.3420201433256622181, 0.9396926207859107594, -6.162975822039141593E-32 ) ) ;
#13862 = CARTESIAN_POINT ( 'NONE',  ( 65.40000000218495302, 9.999999999999998224, 17.49999999999999645 ) ) ;
#13863 = ORIENTED_EDGE ( 'NONE', *, *, #2528, .F. ) ;
#13864 = PLANE ( 'NONE',  #13442 ) ;
#13865 = CARTESIAN_POINT ( 'NONE',  ( -2.449293598294706907E-16, 4.000000000000000000, 4.175000002731186655 ) ) ;
#13866 = ORIENTED_EDGE ( 'NONE', *, *, #17844, .F. ) ;
#13867 = ORIENTED_EDGE ( 'NONE', *, *, #4387, .T. ) ;
#13868 = CARTESIAN_POINT ( 'NONE',  ( 22.11331769071655984, -8.974600000000002353, 10.00000000000008882 ) ) ;
#13869 =( BOUNDED_CURVE ( )  B_SPLINE_CURVE ( 2, ( #4651, #2487, #4299 ),
 .UNSPECIFIED., .F., .F. ) 
 B_SPLINE_CURVE_WITH_KNOTS ( ( 3, 3 ),
 ( 0.9155333511103322941, 0.9235200992307018852 ),
 .UNSPECIFIED. ) 
 CURVE ( )  GEOMETRIC_REPRESENTATION_ITEM ( )  RATIONAL_B_SPLINE_CURVE ( ( 0.9720211172018224932, 0.9469897216464003842, 0.9841097943611590848 ) ) 
 REPRESENTATION_ITEM ( '' )  );
#13870 = CARTESIAN_POINT ( 'NONE',  ( 60.00000000000000711, 15.00000000000000000, 10.00000000000007105 ) ) ;
#13871 = ORIENTED_EDGE ( 'NONE', *, *, #2088, .T. ) ;
#13872 = PLANE ( 'NONE',  #6490 ) ;
#13873 = UNCERTAINTY_MEASURE_WITH_UNIT (LENGTH_MEASURE( 1.000000000000000082E-05 ), #7380, 'distance_accuracy_value', 'NONE');
#13874 = CARTESIAN_POINT ( 'NONE',  ( 67.65000000109247935, 9.999999999999998224, 12.93301269999999192 ) ) ;
#13875 = CARTESIAN_POINT ( 'NONE',  ( 69.00000000109245946, 10.85617417291294551, 17.06698729999999742 ) ) ;
#13876 = ORIENTED_EDGE ( 'NONE', *, *, #8691, .T. ) ;
#13877 = EDGE_CURVE ( 'NONE', #16003, #9531, #11037, .T. ) ;
#13878 = DIRECTION ( 'NONE',  ( -1.000000000000000000, 0.000000000000000000, 0.000000000000000000 ) ) ;
#13879 = CARTESIAN_POINT ( 'NONE',  ( 54.56250000000000711, 5.999999999999996447, 15.00000000000001599 ) ) ;
#13880 = CARTESIAN_POINT ( 'NONE',  ( -1.432654583217640276, 3.458734125000000326, 3.550000001365595459 ) ) ;
#13881 = CARTESIAN_POINT ( 'NONE',  ( -1.432654583217638944, 3.458734125000000326, 17.25000000136560274 ) ) ;
#13882 = CARTESIAN_POINT ( 'NONE',  ( 68.20000000218495018, 9.999999999999998224, 12.49999999999999289 ) ) ;
#13883 = DIRECTION ( 'NONE',  ( 1.000000000000000000, 0.000000000000000000, 0.000000000000000000 ) ) ;
#13884 = ORIENTED_EDGE ( 'NONE', *, *, #13820, .T. ) ;
#13885 = LINE ( 'NONE', #17813, #15716 ) ;
#13886 = FACE_OUTER_BOUND ( 'NONE', #1448, .T. ) ;
#13887 = CARTESIAN_POINT ( 'NONE',  ( 2.000000000000001776, 0.000000000000000000, -8.800000000000023803 ) ) ;
#13888 = EDGE_CURVE ( 'NONE', #11740, #2044, #13329, .T. ) ;
#13889 = ORIENTED_EDGE ( 'NONE', *, *, #10956, .F. ) ;
#13890 = LINE ( 'NONE', #11866, #19433 ) ;
#13891 = CARTESIAN_POINT ( 'NONE',  ( 4.999999999999999112, -7.360373001730951437, 4.729683950898845524 ) ) ;
#13892 = DIRECTION ( 'NONE',  ( 0.000000000000000000, 1.224646799147333486E-16, 1.000000000000000000 ) ) ;
#13893 = ORIENTED_EDGE ( 'NONE', *, *, #13631, .F. ) ;
#13894 = CARTESIAN_POINT ( 'NONE',  ( -19.99999999999999645, -11.25000000000000355, 10.00000000000008882 ) ) ;
#13895 = ORIENTED_EDGE ( 'NONE', *, *, #5397, .T. ) ;
#13896 = CARTESIAN_POINT ( 'NONE',  ( 71.15000000109247935, 11.46158073645647235, 16.46158073645647235 ) ) ;
#13897 = CARTESIAN_POINT ( 'NONE',  ( 70.00000000218494733, 12.50000000000000000, 14.99999999999999645 ) ) ;
#13898 =( BOUNDED_SURFACE ( )  B_SPLINE_SURFACE ( 1, 2, ( 
 ( #7599, #22175, #5790, #3983, #20500, #9642, #11445, #4583, #13474, #4340, #8303, #22414, #7952, #11919, #17405, #2773, #2308, #19187, #11679, #18948, #624, #6383, #15272, #6025, #17292, #2533, #5908, #11566, #8083, #17049, #15393, #9874, #16933, #18718, #22773, #4105, #17169, #13701, #20964, #857, #10113, #973, #15625, #747, #6151, #15153, #22656, #6265, #20735, #22543, #509, #4457, #7832, #4228, #13354, #13234, #13583, #2659, #20621, #18834, #20850, #2420, #11797, #8191, #9751, #19069, #10001, #15504, #21434, #6509, #1319, #4932, #8433, #3247, #19408, #12267, #23370, #4696, #14291, #8543, #10355, #8658, #17645, #6973, #21084, #5048, #23015, #12031, #6737, #3366, #21552, #14044, #15745, #17752, #2885, #19294, #19646, #10710, #6620, #17987, #5164, #12506, #1563, #15850, #10593, #1206, #19764, #8901, #22895, #17522, #12381, #13938, #13828, #10232, #23122, #21309, #19533, #3131, #1089, #10471, #15958, #21196, #4810, #17865, #16082, #12141, #3005, #23239, #6849, #14174, #1439, #8778, #3711, #12972, #9145, #5638, #19995, #14537, #18216, #18452, #3843, #11053, #21910, #21802, #20109, #9372, #21675, #5517, #5767 ),
 ( #16432, #12852, #237, #13, #1920, #9261, #16197, #10825, #11179, #18566, #7454, #23483, #16547, #11291, #7222, #20237, #123, #23607, #14769, #16662, #2031, #14890, #5284, #7571, #12629, #5407, #22023, #22148, #1797, #18340, #3490, #13095, #20350, #2149, #3957, #9024, #7096, #14413, #16317, #12744, #3598, #19889, #18100, #10937, #7345, #1680, #14652, #22510, #9844, #6361, #7922, #22634, #2629, #4316, #5997, #19039, #11770, #15015, #20593, #4077, #11892, #18690, #2394, #20827, #9973, #4200, #11414, #15242, #22387, #597, #9727, #365, #17266, #13324, #2280, #9484, #9618, #19161, #7698, #17140, #16784, #16908, #4436, #22269, #717, #5881, #8053, #4555, #486, #13558, #18924, #7809, #15367, #834, #8166, #15479, #13205, #22749, #20471, #15126, #6238, #13676, #11542, #6120, #18811, #20938, #17022, #13449, #20712, #11655, #2510, #10088, #2859, #22991, #8405, #19511, #3108, #21170, #1064, #4669, #19270, #15825, #10449, #23346, #1185, #15934, #19620, #21283, #6596, #12359, #5028, #8283, #13913, #21058, #5139, #12004, #19382, #14146, #3218, #4783, #10209, #8521, #15721, #17623, #2977, #17377, #10567, #12119, #17497 ) ),
 .UNSPECIFIED., .F., .F., .F. ) 
 B_SPLINE_SURFACE_WITH_KNOTS ( ( 2, 2 ),
 ( 3, 2, 2, 2, 2, 2, 2, 2, 2, 2, 2, 2, 2, 2, 2, 2, 2, 2, 2, 2, 2, 2, 2, 2, 2, 2, 2, 2, 2, 2, 2, 2, 2, 2, 2, 2, 2, 2, 2, 2, 2, 2, 2, 2, 2, 2, 2, 2, 2, 2, 2, 2, 2, 2, 2, 2, 2, 2, 2, 2, 2, 2, 2, 2, 2, 2, 2, 2, 2, 2, 2, 2, 2, 2, 3 ),
 ( 0.000000000000000000, 1.000000000000000000 ),
 ( 0.000000000000000000, 0.01250000000000000069, 0.02500000000000000139, 0.03749999999999999861, 0.05000000000000000278, 0.06250000000000000000, 0.07499999999999999722, 0.08749999999999999445, 0.1000000000000000056, 0.1125000000000000028, 0.1250000000000000000, 0.1375000000000000111, 0.1499999999999999944, 0.1625000000000000056, 0.1749999999999999889, 0.1875000000000000000, 0.2000000000000000111, 0.2124999999999999944, 0.2250000000000000056, 0.2374999999999999889, 0.2500000000000000000, 0.2625000000000000111, 0.2750000000000000222, 0.2874999999999999778, 0.2999999999999999889, 0.3125000000000000000, 0.3250000000000000111, 0.3375000000000000222, 0.3499999999999999778, 0.3624999999999999889, 0.3750000000000000000, 0.3875000000000000111, 0.4000000000000000222, 0.4124999999999999778, 0.4249999999999999889, 0.4375000000000000000, 0.4500000000000000111, 0.4625000000000000222, 0.4749999999999999778, 0.4874999999999999889, 0.5000000000000000000, 0.5124999999999999556, 0.5250000000000000222, 0.5374999999999999778, 0.5500000000000000444, 0.5625000000000000000, 0.5749999999999999556, 0.5875000000000000222, 0.5999999999999999778, 0.6125000000000000444, 0.6250000000000000000, 0.6374999999999999556, 0.6500000000000000222, 0.6624999999999999778, 0.6750000000000000444, 0.6875000000000000000, 0.6999999999999999556, 0.7125000000000000222, 0.7249999999999999778, 0.7375000000000000444, 0.7500000000000000000, 0.7624999999999999556, 0.7750000000000000222, 0.7874999999999999778, 0.8000000000000000444, 0.8125000000000000000, 0.8249999999999999556, 0.8375000000000000222, 0.8499999999999999778, 0.8625000000000000444, 0.8750000000000000000, 0.8874999999999999556, 0.9000000000000000222, 0.9124999999999999778, 0.9250000000000000444 ),
 .UNSPECIFIED. ) 
 GEOMETRIC_REPRESENTATION_ITEM ( )  RATIONAL_B_SPLINE_SURFACE ( (
 ( 1.000000000000000000, 0.9238795325112867385, 1.000000000000000000, 0.9238795325112867385, 1.000000000000000000, 0.9238795325112867385, 1.000000000000000000, 0.9238795325112867385, 1.000000000000000000, 0.9238795325112867385, 1.000000000000000000, 0.9238795325112867385, 1.000000000000000000, 0.9238795325112867385, 1.000000000000000000, 0.9238795325112867385, 1.000000000000000000, 0.9238795325112867385, 1.000000000000000000, 0.9238795325112867385, 1.000000000000000000, 0.9238795325112867385, 1.000000000000000000, 0.9238795325112867385, 1.000000000000000000, 0.9238795325112867385, 1.000000000000000000, 0.9238795325112867385, 1.000000000000000000, 0.9238795325112867385, 1.000000000000000000, 0.9238795325112867385, 1.000000000000000000, 0.9238795325112867385, 1.000000000000000000, 0.9238795325112867385, 1.000000000000000000, 0.9238795325112867385, 1.000000000000000000, 0.9238795325112867385, 1.000000000000000000, 0.9238795325112867385, 1.000000000000000000, 0.9238795325112867385, 1.000000000000000000, 0.9238795325112867385, 1.000000000000000000, 0.9238795325112867385, 1.000000000000000000, 0.9238795325112867385, 1.000000000000000000, 0.9238795325112867385, 1.000000000000000000, 0.9238795325112867385, 1.000000000000000000, 0.9238795325112867385, 1.000000000000000000, 0.9238795325112867385, 1.000000000000000000, 0.9238795325112867385, 1.000000000000000000, 0.9238795325112867385, 1.000000000000000000, 0.9238795325112867385, 1.000000000000000000, 0.9238795325112867385, 1.000000000000000000, 0.9238795325112867385, 1.000000000000000000, 0.9238795325112867385, 1.000000000000000000, 0.9238795325112867385, 1.000000000000000000, 0.9238795325112867385, 1.000000000000000000, 0.9238795325112867385, 1.000000000000000000, 0.9238795325112867385, 1.000000000000000000, 0.9238795325112867385, 1.000000000000000000, 0.9238795325112867385, 1.000000000000000000, 0.9238795325112867385, 1.000000000000000000, 0.9238795325112867385, 1.000000000000000000, 0.9238795325112867385, 1.000000000000000000, 0.9238795325112867385, 1.000000000000000000, 0.9238795325112867385, 1.000000000000000000, 0.9238795325112867385, 1.000000000000000000, 0.9238795325112867385, 1.000000000000000000, 0.9238795325112867385, 1.000000000000000000, 0.9238795325112867385, 1.000000000000000000, 0.9238795325112867385, 1.000000000000000000, 0.9238795325112867385, 1.000000000000000000, 0.9238795325112867385, 1.000000000000000000, 0.9238795325112867385, 1.000000000000000000, 0.9238795325112867385, 1.000000000000000000, 0.9238795325112867385, 1.000000000000000000, 0.9238795325112867385, 1.000000000000000000, 0.9238795325112867385, 1.000000000000000000, 0.9238795325112867385, 1.000000000000000000, 0.9238795325112867385, 1.000000000000000000, 0.9238795325112867385, 1.000000000000000000, 0.9238795325112867385, 1.000000000000000000, 0.9238795325112867385, 1.000000000000000000, 0.9238795325112867385, 1.000000000000000000, 0.9238795325112867385, 1.000000000000000000, 0.9238795325112867385, 1.000000000000000000, 0.9238795325112867385, 1.000000000000000000, 0.9238795325112867385, 1.000000000000000000, 0.9238795325112867385, 1.000000000000000000, 0.9238795325112867385, 1.000000000000000000, 0.9238795325112867385, 1.000000000000000000, 0.9238795325112867385, 1.000000000000000000, 0.9238795325112867385, 1.000000000000000000, 0.9238795325112867385, 1.000000000000000000),
 ( 1.000000000000000000, 0.9238795325112867385, 1.000000000000000000, 0.9238795325112867385, 1.000000000000000000, 0.9238795325112867385, 1.000000000000000000, 0.9238795325112867385, 1.000000000000000000, 0.9238795325112867385, 1.000000000000000000, 0.9238795325112867385, 1.000000000000000000, 0.9238795325112867385, 1.000000000000000000, 0.9238795325112867385, 1.000000000000000000, 0.9238795325112867385, 1.000000000000000000, 0.9238795325112867385, 1.000000000000000000, 0.9238795325112867385, 1.000000000000000000, 0.9238795325112867385, 1.000000000000000000, 0.9238795325112867385, 1.000000000000000000, 0.9238795325112867385, 1.000000000000000000, 0.9238795325112867385, 1.000000000000000000, 0.9238795325112867385, 1.000000000000000000, 0.9238795325112867385, 1.000000000000000000, 0.9238795325112867385, 1.000000000000000000, 0.9238795325112867385, 1.000000000000000000, 0.9238795325112867385, 1.000000000000000000, 0.9238795325112867385, 1.000000000000000000, 0.9238795325112867385, 1.000000000000000000, 0.9238795325112867385, 1.000000000000000000, 0.9238795325112867385, 1.000000000000000000, 0.9238795325112867385, 1.000000000000000000, 0.9238795325112867385, 1.000000000000000000, 0.9238795325112867385, 1.000000000000000000, 0.9238795325112867385, 1.000000000000000000, 0.9238795325112867385, 1.000000000000000000, 0.9238795325112867385, 1.000000000000000000, 0.9238795325112867385, 1.000000000000000000, 0.9238795325112867385, 1.000000000000000000, 0.9238795325112867385, 1.000000000000000000, 0.9238795325112867385, 1.000000000000000000, 0.9238795325112867385, 1.000000000000000000, 0.9238795325112867385, 1.000000000000000000, 0.9238795325112867385, 1.000000000000000000, 0.9238795325112867385, 1.000000000000000000, 0.9238795325112867385, 1.000000000000000000, 0.9238795325112867385, 1.000000000000000000, 0.9238795325112867385, 1.000000000000000000, 0.9238795325112867385, 1.000000000000000000, 0.9238795325112867385, 1.000000000000000000, 0.9238795325112867385, 1.000000000000000000, 0.9238795325112867385, 1.000000000000000000, 0.9238795325112867385, 1.000000000000000000, 0.9238795325112867385, 1.000000000000000000, 0.9238795325112867385, 1.000000000000000000, 0.9238795325112867385, 1.000000000000000000, 0.9238795325112867385, 1.000000000000000000, 0.9238795325112867385, 1.000000000000000000, 0.9238795325112867385, 1.000000000000000000, 0.9238795325112867385, 1.000000000000000000, 0.9238795325112867385, 1.000000000000000000, 0.9238795325112867385, 1.000000000000000000, 0.9238795325112867385, 1.000000000000000000, 0.9238795325112867385, 1.000000000000000000, 0.9238795325112867385, 1.000000000000000000, 0.9238795325112867385, 1.000000000000000000, 0.9238795325112867385, 1.000000000000000000, 0.9238795325112867385, 1.000000000000000000, 0.9238795325112867385, 1.000000000000000000, 0.9238795325112867385, 1.000000000000000000, 0.9238795325112867385, 1.000000000000000000, 0.9238795325112867385, 1.000000000000000000, 0.9238795325112867385, 1.000000000000000000, 0.9238795325112867385, 1.000000000000000000, 0.9238795325112867385, 1.000000000000000000, 0.9238795325112867385, 1.000000000000000000, 0.9238795325112867385, 1.000000000000000000, 0.9238795325112867385, 1.000000000000000000, 0.9238795325112867385, 1.000000000000000000, 0.9238795325112867385, 1.000000000000000000, 0.9238795325112867385, 1.000000000000000000) ) ) 
 REPRESENTATION_ITEM ( '' )  SURFACE ( )  );
#13899 = CARTESIAN_POINT ( 'NONE',  ( -19.99999999999999645, -9.000000000000003553, 5.000000000000079936 ) ) ;
#13900 = CARTESIAN_POINT ( 'NONE',  ( 3.254516946766202512, -9.000000000000001776, 10.00000000000008882 ) ) ;
#13901 = CARTESIAN_POINT ( 'NONE',  ( 65.95000000109246230, 8.538419263543522320, 16.46158073645647235 ) ) ;
#13902 = VERTEX_POINT ( 'NONE', #4773 ) ;
#13903 = EDGE_CURVE ( 'NONE', #7993, #3902, #1816, .T. ) ;
#13904 = DIRECTION ( 'NONE',  ( -1.000000000000000000, -0.000000000000000000, -0.000000000000000000 ) ) ;
#13905 = EDGE_CURVE ( 'NONE', #15228, #17794, #8512, .T. ) ;
#13906 = DIRECTION ( 'NONE',  ( -1.224646799147353207E-16, 0.000000000000000000, -1.000000000000000000 ) ) ;
#13907 = CARTESIAN_POINT ( 'NONE',  ( 70.40000000109247935, 12.06698730000000275, 14.14382582708705094 ) ) ;
#13908 = CARTESIAN_POINT ( 'NONE',  ( -3.458734124999999437, 1.432654583217640498, 19.62500000136560629 ) ) ;
#13909 = CARTESIAN_POINT ( 'NONE',  ( 45.52901028033275566, -11.25000000000000355, 5.000000000000079936 ) ) ;
#13910 = AXIS2_PLACEMENT_3D ( 'NONE', #15599, #1293, #1409 ) ;
#13911 = CARTESIAN_POINT ( 'NONE',  ( 6.499999999999999112, 3.145973671264227889, -0.4053876232513715649 ) ) ;
#13912 = ORIENTED_EDGE ( 'NONE', *, *, #20892, .F. ) ;
#13913 = CARTESIAN_POINT ( 'NONE',  ( -2.449293598294706907E-16, 4.000000000000000000, -1.949999999999998623 ) ) ;
#13914 = AXIS2_PLACEMENT_3D ( 'NONE', #10211, #8408, #9975 ) ;
#13915 = DIRECTION ( 'NONE',  ( -1.000000000000000000, 0.000000000000000000, 0.000000000000000000 ) ) ;
#13916 = CARTESIAN_POINT ( 'NONE',  ( 0.000000000000000000, 0.000000000000000000, 3.469446951953614189E-15 ) ) ;
#13917 = DIRECTION ( 'NONE',  ( -0.3420201433256622181, 0.9396926207859106484, 1.232595164407828100E-31 ) ) ;
#13918 = EDGE_CURVE ( 'NONE', #18283, #7307, #11699, .T. ) ;
#13919 = ORIENTED_EDGE ( 'NONE', *, *, #15985, .T. ) ;
#13920 = CARTESIAN_POINT ( 'NONE',  ( 1.656854249492384135, -3.999999999999999112, 13.43750000273119838 ) ) ;
#13921 = ORIENTED_EDGE ( 'NONE', *, *, #12495, .F. ) ;
#13922 = CARTESIAN_POINT ( 'NONE',  ( -66.10000000109246798, 7.933012699999995476, 14.14382582708705094 ) ) ;
#13923 = CONTEXT_DEPENDENT_SHAPE_REPRESENTATION ( #14072, #16788 ) ;
#13924 = EDGE_LOOP ( 'NONE', ( #19801, #4910, #21835, #22377 ) ) ;
#13925 = DIRECTION ( 'NONE',  ( -1.000000000000000000, -0.000000000000000000, -0.000000000000000000 ) ) ;
#13926 = VERTEX_POINT ( 'NONE', #21271 ) ;
#13927 = ORIENTED_EDGE ( 'NONE', *, *, #16782, .F. ) ;
#13928 = CARTESIAN_POINT ( 'NONE',  ( -1.432654583217639832, -3.458734125000000326, 12.87500000136560629 ) ) ;
#13929 = LINE ( 'NONE', #8536, #14968 ) ;
#13930 = AXIS2_PLACEMENT_3D ( 'NONE', #3649, #13026, #16483 ) ;
#13931 = DIRECTION ( 'NONE',  ( 0.3420201433256622181, 0.9396926207859107594, -6.162975822039141593E-32 ) ) ;
#13932 = EDGE_CURVE ( 'NONE', #23556, #6771, #17254, .T. ) ;
#13933 = CARTESIAN_POINT ( 'NONE',  ( 65.80000000109247082, 7.933012699999995476, 15.85617417291294196 ) ) ;
#13934 = CARTESIAN_POINT ( 'NONE',  ( -70.20000000000000284, 8.232233047033627571, 16.76776695296636532 ) ) ;
#13935 = EDGE_CURVE ( 'NONE', #4844, #19360, #23333, .T. ) ;
#13936 = CARTESIAN_POINT ( 'NONE',  ( 6.499999999999999112, -1.264206540070616835, -0.05450957050772529261 ) ) ;
#13937 = CARTESIAN_POINT ( 'NONE',  ( 60.00000000000000711, 11.02940789746247141, 18.43681100577745013 ) ) ;
#13938 = CARTESIAN_POINT ( 'NONE',  ( -3.458734125000000326, -1.432654583217642497, -0.9499999986344030978 ) ) ;
#13939 = CARTESIAN_POINT ( 'NONE',  ( 10.15255810323380992, -9.000000000000001776, 5.000000000000079936 ) ) ;
#13940 = CARTESIAN_POINT ( 'NONE',  ( 71.45000000000000284, 12.50000000000000000, 13.96446609406725692 ) ) ;
#13941 = CARTESIAN_POINT ( 'NONE',  ( 4.000000000000000888, 4.898587196589412829E-16, 11.62500000273119660 ) ) ;
#13942 = CARTESIAN_POINT ( 'NONE',  ( 50.00000000000000000, -15.00000000000003375, 34.11836509645780779 ) ) ;
#13943 = EDGE_CURVE ( 'NONE', #2142, #15640, #16371, .T. ) ;
#13944 = EDGE_CURVE ( 'NONE', #20363, #6074, #18294, .T. ) ;
#13945 = EDGE_LOOP ( 'NONE', ( #23623, #8123, #6625, #16616 ) ) ;
#13946 = CARTESIAN_POINT ( 'NONE',  ( 0.9413949561959078505, 0.3373062947069096484, 10.00000000000000888 ) ) ;
#13947 = ORIENTED_EDGE ( 'NONE', *, *, #19977, .T. ) ;
#13948 = CARTESIAN_POINT ( 'NONE',  ( 60.52893183416158251, 11.58880310854676132, 19.02818770551463956 ) ) ;
#13949 = CARTESIAN_POINT ( 'NONE',  ( -71.55000000109247082, 8.538419263543524096, 13.53841926354352054 ) ) ;
#13950 = CARTESIAN_POINT ( 'NONE',  ( -1.432654583217640276, 3.458734125000000326, 1.550000001365597013 ) ) ;
#13951 = ORIENTED_EDGE ( 'NONE', *, *, #6502, .T. ) ;
#13952 = DIRECTION ( 'NONE',  ( 1.224646799147353207E-16, 1.000000000000000000, 0.000000000000000000 ) ) ;
#13953 = ORIENTED_EDGE ( 'NONE', *, *, #316, .F. ) ;
#13954 = CARTESIAN_POINT ( 'NONE',  ( -3.999999999999999112, 0.000000000000000000, 20.00000000000001066 ) ) ;
#13955 = VERTEX_POINT ( 'NONE', #19727 ) ;
#13956 = CARTESIAN_POINT ( 'NONE',  ( 57.40856816583844591, 12.97181229448534978, 13.68930817193506755 ) ) ;
#13957 = CARTESIAN_POINT ( 'NONE',  ( -66.25000000218494733, 8.964466094067258695, 17.50000000000000355 ) ) ;
#13958 = DIRECTION ( 'NONE',  ( -1.000000000000000000, -0.000000000000000000, -0.000000000000000000 ) ) ;
#13959 = CARTESIAN_POINT ( 'NONE',  ( -71.80000000109245661, 9.143825827087050939, 12.93301269999999370 ) ) ;
#13960 = CARTESIAN_POINT ( 'NONE',  ( -2.445694354108819191, 2.445694354108820523, 17.56250000136560274 ) ) ;
#13961 = CARTESIAN_POINT ( 'NONE',  ( -3.999999999999999112, 1.656854249492380804, 14.06250000273119660 ) ) ;
#13962 = CARTESIAN_POINT ( 'NONE',  ( 57.56250000000000000, 6.999999999999997335, 15.00000000000000533 ) ) ;
#13963 = CARTESIAN_POINT ( 'NONE',  ( 69.15000000109247935, 8.538419263543524096, 13.53841926354352054 ) ) ;
#13964 = CARTESIAN_POINT ( 'NONE',  ( 70.75000000218496155, 12.50000000000000000, 13.96446609406725692 ) ) ;
#13965 = CARTESIAN_POINT ( 'NONE',  ( 57.75000000000000000, 7.878679656440361612, 17.12132034355964549 ) ) ;
#13966 = CARTESIAN_POINT ( 'NONE',  ( 3.458734125000001214, -1.432654583217639610, 0.4250000013655961251 ) ) ;
#13967 = CARTESIAN_POINT ( 'NONE',  ( 67.65000000218496723, 12.50000000000000000, 16.03553390593273775 ) ) ;
#13968 = ADVANCED_FACE ( 'NONE', ( #17828 ), #21638, .F. ) ;
#13969 = CARTESIAN_POINT ( 'NONE',  ( -68.85000000109246798, 12.06698730000000097, 14.99999999999999645 ) ) ;
#13970 = EDGE_CURVE ( 'NONE', #12520, #23136, #14494, .T. ) ;
#13971 = ORIENTED_EDGE ( 'NONE', *, *, #4996, .T. ) ;
#13972 = DIRECTION ( 'NONE',  ( -1.000000000000000000, 0.000000000000000000, 0.000000000000000000 ) ) ;
#13973 = CARTESIAN_POINT ( 'NONE',  ( 65.45000000218495018, 8.964466094067260471, 17.50000000000000355 ) ) ;
#13974 = ORIENTED_EDGE ( 'NONE', *, *, #12990, .F. ) ;
#13975 = CARTESIAN_POINT ( 'NONE',  ( 59.34375000000000711, 8.757359312880723223, 18.00000000000000355 ) ) ;
#13976 = VECTOR ( 'NONE', #17206, 1000.000000000000000 ) ;
#13977 = CARTESIAN_POINT ( 'NONE',  ( -2.828427124746189403, -2.828427124746190735, 0.5500000027311869877 ) ) ;
#13978 = VECTOR ( 'NONE', #23208, 1000.000000000000114 ) ;
#13979 = ORIENTED_EDGE ( 'NONE', *, *, #11754, .T. ) ;
#13980 = ORIENTED_EDGE ( 'NONE', *, *, #12915, .F. ) ;
#13981 = CARTESIAN_POINT ( 'NONE',  ( -66.90000000000000568, 9.999999999999998224, 17.49999999999999645 ) ) ;
#13982 = ORIENTED_EDGE ( 'NONE', *, *, #3205, .T. ) ;
#13983 = FACE_OUTER_BOUND ( 'NONE', #2724, .T. ) ;
#13984 = FACE_OUTER_BOUND ( 'NONE', #17376, .T. ) ;
#13985 = CARTESIAN_POINT ( 'NONE',  ( 67.85000000109246798, 9.999999999999998224, 12.93301269999999192 ) ) ;
#13986 = CIRCLE ( 'NONE', #21983, 2.500000000000007550 ) ;
#13987 = CYLINDRICAL_SURFACE ( 'NONE', #2817, 4.000000000000000000 ) ;
#13988 = PLANE ( 'NONE',  #4964 ) ;
#13989 = CARTESIAN_POINT ( 'NONE',  ( 51.65625000000000711, 6.000000000000004441, 16.65685424949239390 ) ) ;
#13990 = CARTESIAN_POINT ( 'NONE',  ( 3.458734125000000326, 4.235727675282971730E-16, 4.237500001365595459 ) ) ;
#13991 = CARTESIAN_POINT ( 'NONE',  ( 2.445694354108821855, -2.445694354108820079, 14.81250000136560452 ) ) ;
#13992 = CARTESIAN_POINT ( 'NONE',  ( 0.000000000000000000, 0.000000000000000000, 19.04999999999996874 ) ) ;
#13993 = DIRECTION ( 'NONE',  ( 0.3420201433256622736, -0.9396926207859106484, -1.232595164407828100E-31 ) ) ;
#13994 = EDGE_LOOP ( 'NONE', ( #2952, #8373, #15336, #4521, #17033, #4642 ) ) ;
#13995 = CARTESIAN_POINT ( 'NONE',  ( -20.00005080000000035, 0.000000000000000000, -6.000000000000000888 ) ) ;
#13996 =( BOUNDED_CURVE ( )  B_SPLINE_CURVE ( 2, ( #22733, #21154, #10314, #17602, #19019, #4655, #1049, #2491, #6345 ),
 .UNSPECIFIED., .F., .F. ) 
 B_SPLINE_CURVE_WITH_KNOTS ( ( 3, 2, 2, 2, 3 ),
 ( 0.2000000000000000111, 0.2124999999999999944, 0.2250000000000000056, 0.2374999999999999889, 0.2500000000000000000 ),
 .UNSPECIFIED. ) 
 CURVE ( )  GEOMETRIC_REPRESENTATION_ITEM ( )  RATIONAL_B_SPLINE_CURVE ( ( 1.000000000000000000, 0.9238795325112867385, 1.000000000000000000, 0.9238795325112867385, 1.000000000000000000, 0.9238795325112867385, 1.000000000000000000, 0.9238795325112867385, 1.000000000000000000 ) ) 
 REPRESENTATION_ITEM ( '' )  );
#13997 = CARTESIAN_POINT ( 'NONE',  ( 0.000000000000000000, 0.000000000000000000, -3.700000000000000178 ) ) ;
#13998 = CARTESIAN_POINT ( 'NONE',  ( 4.000000000000000000, 4.898587196589412829E-16, -1.199999999999997957 ) ) ;
#13999 = VERTEX_POINT ( 'NONE', #8989 ) ;
#14000 = CARTESIAN_POINT ( 'NONE',  ( 2.499999999999999556, 9.680994141368849171, -5.222868219166749704 ) ) ;
#14001 = DIRECTION ( 'NONE',  ( 0.000000000000000000, 0.000000000000000000, 1.000000000000000000 ) ) ;
#14002 = AXIS2_PLACEMENT_3D ( 'NONE', #20145, #9296, #2069 ) ;
#14003 = AXIS2_PLACEMENT_3D ( 'NONE', #5463, #1263, #8717 ) ;
#14004 = DIRECTION ( 'NONE',  ( -0.9396926207859107594, -0.3420201433256623291, 1.540743955509804830E-32 ) ) ;
#14005 = VERTEX_POINT ( 'NONE', #19608 ) ;
#14006 = CARTESIAN_POINT ( 'NONE',  ( 0.000000000000000000, 0.000000000000000000, 9.480888224575631185 ) ) ;
#14007 = ORIENTED_EDGE ( 'NONE', *, *, #22075, .F. ) ;
#14008 = ADVANCED_FACE ( 'NONE', ( #16043 ), #7055, .F. ) ;
#14009 = CARTESIAN_POINT ( 'NONE',  ( 53.90625000000000000, 13.99999999999999289, 13.34314575050759544 ) ) ;
#14010 = CARTESIAN_POINT ( 'NONE',  ( -3.999999999999999112, 0.000000000000000000, 13.00000000000001066 ) ) ;
#14011 = DIRECTION ( 'NONE',  ( 0.000000000000000000, 0.000000000000000000, 1.000000000000000000 ) ) ;
#14012 = CARTESIAN_POINT ( 'NONE',  ( 4.000000000000000888, 4.898587196589412829E-16, 11.50000000000001066 ) ) ;
#14013 = CARTESIAN_POINT ( 'NONE',  ( 66.00000000109245946, 7.933012699999995476, 15.85617417291294196 ) ) ;
#14014 = ORIENTED_EDGE ( 'NONE', *, *, #6702, .F. ) ;
#14015 = CARTESIAN_POINT ( 'NONE',  ( -68.80000000218494449, 7.499999999999996447, 14.99999999999999645 ) ) ;
#14016 = CARTESIAN_POINT ( 'NONE',  ( -4.000000000000000000, -1.656854249492383024, -1.512499997268811347 ) ) ;
#14017 = CARTESIAN_POINT ( 'NONE',  ( 66.80000000109247082, 7.933012699999995476, 15.85617417291294196 ) ) ;
#14018 = CARTESIAN_POINT ( 'NONE',  ( -3.458734124999998993, -1.432654583217642497, 18.75000000136560274 ) ) ;
#14019 = CARTESIAN_POINT ( 'NONE',  ( -35.00000000000000711, 1.500000000000003109, -49.99999999999999289 ) ) ;
#14020 = DIRECTION ( 'NONE',  ( -1.000000000000000000, 0.000000000000000000, 0.000000000000000000 ) ) ;
#14021 = ORIENTED_EDGE ( 'NONE', *, *, #9693, .T. ) ;
#14022 = LINE ( 'NONE', #4907, #7026 ) ;
#14023 = CARTESIAN_POINT ( 'NONE',  ( -3.999999999999999112, 0.000000000000000000, 16.00000000000001066 ) ) ;
#14024 = CARTESIAN_POINT ( 'NONE',  ( 2.500000000000000000, 1.178949249685217415, 2.041999999999998483 ) ) ;
#14025 = VERTEX_POINT ( 'NONE', #18065 ) ;
#14026 = PLANE ( 'NONE',  #175 ) ;
#14027 = EDGE_LOOP ( 'NONE', ( #8672, #14753, #14512, #928, #3010, #16181, #2779, #12187 ) ) ;
#14028 = CARTESIAN_POINT ( 'NONE',  ( -6.500000000000000888, 1.277696550142688459, -0.05601745114479440152 ) ) ;
#14029 = EDGE_LOOP ( 'NONE', ( #1456, #14356, #3937, #2188 ) ) ;
#14030 = CARTESIAN_POINT ( 'NONE',  ( 2.000000000000005329, -3.464101615137751722, 0.000000000000000000 ) ) ;
#14031 = ORIENTED_EDGE ( 'NONE', *, *, #22166, .F. ) ;
#14032 = ADVANCED_FACE ( 'NONE', ( #3453 ), #16506, .T. ) ;
#14033 = EDGE_CURVE ( 'NONE', #13655, #14025, #3325, .T. ) ;
#14034 = ORIENTED_EDGE ( 'NONE', *, *, #12020, .F. ) ;
#14035 = CARTESIAN_POINT ( 'NONE',  ( 1.025207404391860050E-15, 3.458734125000000770, 12.43750000136560629 ) ) ;
#14036 = DIRECTION ( 'NONE',  ( -0.000000000000000000, -0.000000000000000000, 1.000000000000000000 ) ) ;
#14037 = CARTESIAN_POINT ( 'NONE',  ( -66.70000000218495018, 11.76776695296636888, 13.23223304703362579 ) ) ;
#14038 = CARTESIAN_POINT ( 'NONE',  ( 66.55000000109247082, 8.538419263543522320, 16.46158073645647235 ) ) ;
#14039 = EDGE_CURVE ( 'NONE', #11744, #18480, #6508, .T. ) ;
#14040 = CARTESIAN_POINT ( 'NONE',  ( -68.84999999999999432, 8.964466094067258695, 12.49999999999999289 ) ) ;
#14041 = DIRECTION ( 'NONE',  ( -1.000000000000000000, -7.703719777548943412E-32, 0.000000000000000000 ) ) ;
#14042 = CARTESIAN_POINT ( 'NONE',  ( 60.00000000000002842, 13.36943630122111415, 16.95040930672855595 ) ) ;
#14043 = CIRCLE ( 'NONE', #13286, 6.200000000000021494 ) ;
#14044 = CARTESIAN_POINT ( 'NONE',  ( 1.432654583217642275, -3.458734124999999882, 0.3000000013655960696 ) ) ;
#14045 = CARTESIAN_POINT ( 'NONE',  ( 2.828427124746192067, -2.828427124746189847, 13.37500000000001243 ) ) ;
#14046 = CARTESIAN_POINT ( 'NONE',  ( 34.99999999999999289, 7.500000000000001776, -50.00000000000000000 ) ) ;
#14047 = CARTESIAN_POINT ( 'NONE',  ( 3.458734125000002102, -1.432654583217639610, 15.87500000136560807 ) ) ;
#14048 = LINE ( 'NONE', #19893, #6895 ) ;
#14049 = ORIENTED_EDGE ( 'NONE', *, *, #15142, .T. ) ;
#14050 = CARTESIAN_POINT ( 'NONE',  ( -1.656854249492380138, -3.999999999999999112, 14.31250000273119660 ) ) ;
#14051 = ORIENTED_EDGE ( 'NONE', *, *, #9186, .T. ) ;
#14052 = CARTESIAN_POINT ( 'NONE',  ( 53.21643183416158251, 12.97181229448535689, 16.31069182806490758 ) ) ;
#14053 = CARTESIAN_POINT ( 'NONE',  ( -68.10000000109246798, 9.143825827087049163, 17.06698729999999742 ) ) ;
#14054 = FILL_AREA_STYLE_COLOUR ( '', #11818 ) ;
#14055 = EDGE_CURVE ( 'NONE', #18107, #12101, #8734, .T. ) ;
#14056 = CARTESIAN_POINT ( 'NONE',  ( 50.00000000000000000, 2.399706452296353820, 60.00000000000021316 ) ) ;
#14057 = ORIENTED_EDGE ( 'NONE', *, *, #11282, .T. ) ;
#14058 = VECTOR ( 'NONE', #7899, 1000.000000000000000 ) ;
#14059 = AXIS2_PLACEMENT_3D ( 'NONE', #3297, #10639, #18382 ) ;
#14060 = DIRECTION ( 'NONE',  ( 0.000000000000000000, -0.9510565162951565288, 0.3090169943749382364 ) ) ;
#14061 = EDGE_CURVE ( 'NONE', #14828, #5147, #10670, .T. ) ;
#14062 = EDGE_CURVE ( 'NONE', #16322, #5065, #8867, .T. ) ;
#14063 = VERTEX_POINT ( 'NONE', #1760 ) ;
#14064 = LINE ( 'NONE', #12398, #10297 ) ;
#14065 = ORIENTED_EDGE ( 'NONE', *, *, #17611, .T. ) ;
#14066 = CARTESIAN_POINT ( 'NONE',  ( 55.72106816583844591, 13.02818770551464489, 16.17458954617363531 ) ) ;
#14067 = AXIS2_PLACEMENT_3D ( 'NONE', #21702, #21462, #19795 ) ;
#14068 = CARTESIAN_POINT ( 'NONE',  ( -67.45000000218493597, 11.03553390593273598, 12.49999999999999289 ) ) ;
#14069 = EDGE_CURVE ( 'NONE', #5065, #5121, #9127, .T. ) ;
#14070 = CARTESIAN_POINT ( 'NONE',  ( -10.00000000000000000, 0.000000000000000000, 0.000000000000000000 ) ) ;
#14071 = EDGE_CURVE ( 'NONE', #20787, #7410, #3564, .T. ) ;
#14072 =( REPRESENTATION_RELATIONSHIP ('NONE','NONE', #8403, #6707 ) REPRESENTATION_RELATIONSHIP_WITH_TRANSFORMATION ( #4325 )SHAPE_REPRESENTATION_RELATIONSHIP( ) );
#14073 = AXIS2_PLACEMENT_3D ( 'NONE', #17773, #8807, #19788 ) ;
#14074 = DIRECTION ( 'NONE',  ( -1.000000000000000000, 0.000000000000000000, 0.000000000000000000 ) ) ;
#14075 = CARTESIAN_POINT ( 'NONE',  ( -2.445694354108819191, 2.445694354108820523, 14.56250000136560452 ) ) ;
#14076 = CARTESIAN_POINT ( 'NONE',  ( 4.000000000000000888, 4.898587196589412829E-16, 10.62500000273119660 ) ) ;
#14077 = CARTESIAN_POINT ( 'NONE',  ( 17.25467643033275067, -11.25000000000000355, 5.000000000000079936 ) ) ;
#14078 = CIRCLE ( 'NONE', #8722, 8.073750000000021743 ) ;
#14079 = CARTESIAN_POINT ( 'NONE',  ( 4.999999999999999112, -1.239665997526817165, -9.314797388894906049 ) ) ;
#14080 = CARTESIAN_POINT ( 'NONE',  ( 50.47106816583844591, 6.971812294485350670, 13.82541045382635403 ) ) ;
#14081 = CARTESIAN_POINT ( 'NONE',  ( 2.445694354108820079, 2.445694354108820523, -0.3874999986344038194 ) ) ;
#14082 = CARTESIAN_POINT ( 'NONE',  ( 1.656854249492384135, -3.999999999999999112, 18.43750000273119483 ) ) ;
#14083 = CARTESIAN_POINT ( 'NONE',  ( 67.59999999999999432, 11.76776695296636888, 16.76776695296636532 ) ) ;
#14084 = EDGE_LOOP ( 'NONE', ( #230, #17933, #22462, #23314 ) ) ;
#14085 = DIRECTION ( 'NONE',  ( 0.000000000000000000, 0.000000000000000000, 1.000000000000000000 ) ) ;
#14086 = CARTESIAN_POINT ( 'NONE',  ( 65.00000000000000000, 9.999999999999998224, 24.99999999999999645 ) ) ;
#14087 = ORIENTED_EDGE ( 'NONE', *, *, #12662, .T. ) ;
#14088 = CARTESIAN_POINT ( 'NONE',  ( 58.12500000000000000, 12.12132034355964727, 17.12132034355963484 ) ) ;
#14089 =( NAMED_UNIT ( * ) SI_UNIT ( $, .STERADIAN. ) SOLID_ANGLE_UNIT ( ) );
#14090 = CARTESIAN_POINT ( 'NONE',  ( -2.828427124746189403, -2.828427124746190735, -1.449999997268811347 ) ) ;
#14091 = VERTEX_POINT ( 'NONE', #18179 ) ;
#14092 = ORIENTED_EDGE ( 'NONE', *, *, #12185, .F. ) ;
#14093 = AXIS2_PLACEMENT_3D ( 'NONE', #4254, #15529, #22677 ) ;
#14094 = EDGE_CURVE ( 'NONE', #7617, #15752, #5126, .T. ) ;
#14095 = CARTESIAN_POINT ( 'NONE',  ( 4.999999999999999112, 8.264486777890107660, -4.472189673936815879 ) ) ;
#14096 = EDGE_LOOP ( 'NONE', ( #19160, #18871, #6669, #6699 ) ) ;
#14097 = FILL_AREA_STYLE ('',( #21362 ) ) ;
#14098 = VECTOR ( 'NONE', #19341, 1000.000000000000000 ) ;
#14099 = UNCERTAINTY_MEASURE_WITH_UNIT (LENGTH_MEASURE( 1.000000000000000082E-05 ), #7258, 'distance_accuracy_value', 'NONE');
#14100 = CIRCLE ( 'NONE', #7213, 4.000000000000000000 ) ;
#14101 = CARTESIAN_POINT ( 'NONE',  ( 4.000000000000001776, -1.656854249492379694, 11.43750000000001066 ) ) ;
#14102 = ADVANCED_FACE ( 'NONE', ( #20674 ), #6075, .F. ) ;
#14103 = STYLED_ITEM ( 'NONE', ( #518 ), #8790 ) ;
#14104 = EDGE_CURVE ( 'NONE', #18482, #21534, #21987, .T. ) ;
#14105 = DIRECTION ( 'NONE',  ( -1.000000000000000000, 0.000000000000000000, 0.000000000000000000 ) ) ;
#14106 = EDGE_CURVE ( 'NONE', #14872, #4634, #1989, .T. ) ;
#14107 = CARTESIAN_POINT ( 'NONE',  ( 72.09999999999999432, 9.999999999999998224, 12.49999999999999289 ) ) ;
#14108 = CARTESIAN_POINT ( 'NONE',  ( 4.000000000000000888, 4.898587196589412829E-16, 17.62500000273119483 ) ) ;
#14109 = CIRCLE ( 'NONE', #3752, 0.5155456020628804703 ) ;
#14110 = CARTESIAN_POINT ( 'NONE',  ( 28.39650299071657003, -8.974600000000002353, 5.000000000000079936 ) ) ;
#14111 = CARTESIAN_POINT ( 'NONE',  ( 55.15856816583844591, 6.028187705514649330, 16.72490539043803182 ) ) ;
#14112 = CARTESIAN_POINT ( 'NONE',  ( 3.458734125000000326, 4.235727675282971730E-16, 2.237500001365596791 ) ) ;
#14113 = CARTESIAN_POINT ( 'NONE',  ( -1.432654583217639610, -3.458734124999999882, 14.62500000136560452 ) ) ;
#14114 = CARTESIAN_POINT ( 'NONE',  ( 72.50000000000000000, 9.999999999999998224, 14.99999999999999645 ) ) ;
#14115 = AXIS2_PLACEMENT_3D ( 'NONE', #17115, #8258, #22612 ) ;
#14116 = FACE_OUTER_BOUND ( 'NONE', #20027, .T. ) ;
#14117 = ORIENTED_EDGE ( 'NONE', *, *, #17317, .T. ) ;
#14118 = CARTESIAN_POINT ( 'NONE',  ( -1.777000578867806491, 3.418741587802790693, 2.039999999999996927 ) ) ;
#14119 = VECTOR ( 'NONE', #23444, 1000.000000000000000 ) ;
#14120 = CARTESIAN_POINT ( 'NONE',  ( 68.20000000000000284, 11.76776695296636888, 13.23223304703362579 ) ) ;
#14121 = CARTESIAN_POINT ( 'NONE',  ( 1.656854249492383024, -3.999999999999999112, -1.387499999999997735 ) ) ;
#14122 = VERTEX_POINT ( 'NONE', #20310 ) ;
#14123 = FACE_OUTER_BOUND ( 'NONE', #21033, .T. ) ;
#14124 = CARTESIAN_POINT ( 'NONE',  ( 71.95000000109247651, 11.46158073645647235, 16.46158073645647235 ) ) ;
#14125 = CARTESIAN_POINT ( 'NONE',  ( 19.57733605323380743, -9.000000000000001776, 5.000000000000079936 ) ) ;
#14126 = ORIENTED_EDGE ( 'NONE', *, *, #9243, .T. ) ;
#14127 = CARTESIAN_POINT ( 'NONE',  ( 66.20000000218495018, 9.999999999999998224, 17.49999999999999645 ) ) ;
#14128 = ORIENTED_EDGE ( 'NONE', *, *, #22864, .F. ) ;
#14129 = VECTOR ( 'NONE', #6877, 1000.000000000000000 ) ;
#14130 = CARTESIAN_POINT ( 'NONE',  ( 53.81250000000000711, 14.00000000000000000, 14.99999999999997691 ) ) ;
#14131 = ADVANCED_FACE ( 'NONE', ( #18646 ), #7422, .T. ) ;
#14132 = CARTESIAN_POINT ( 'NONE',  ( 67.25000000218494733, 7.499999999999995559, 13.96446609406725692 ) ) ;
#14133 = CARTESIAN_POINT ( 'NONE',  ( 1.656854249492384135, -3.999999999999999112, 16.31250000000001066 ) ) ;
#14134 = DIRECTION ( 'NONE',  ( -1.000000000000000000, -7.703719777548943412E-32, 0.000000000000000000 ) ) ;
#14135 = CARTESIAN_POINT ( 'NONE',  ( 67.20000000109246230, 12.06698729999999919, 14.14382582708705094 ) ) ;
#14136 = VERTEX_POINT ( 'NONE', #23036 ) ;
#14137 = CARTESIAN_POINT ( 'NONE',  ( -20.00000000000001066, 4.500000000000003553, -50.00000000000000000 ) ) ;
#14138 =( BOUNDED_CURVE ( )  B_SPLINE_CURVE ( 2, ( #6211, #19358, #2480 ),
 .UNSPECIFIED., .F., .F. ) 
 B_SPLINE_CURVE_WITH_KNOTS ( ( 3, 3 ),
 ( 0.9000000000000000222, 0.9098660637381802418 ),
 .UNSPECIFIED. ) 
 CURVE ( )  GEOMETRIC_REPRESENTATION_ITEM ( )  RATIONAL_B_SPLINE_CURVE ( ( 1.000000000000000000, 0.9399192492781022201, 0.9746801811257985726 ) ) 
 REPRESENTATION_ITEM ( '' )  );
#14139 = PLANE ( 'NONE',  #12236 ) ;
#14140 = CARTESIAN_POINT ( 'NONE',  ( 66.00000000109245946, 7.933012699999995476, 15.85617417291294196 ) ) ;
#14141 = CARTESIAN_POINT ( 'NONE',  ( 2.445694354108821411, 2.445694354108820523, 19.31250000136560629 ) ) ;
#14142 = FACE_OUTER_BOUND ( 'NONE', #1055, .T. ) ;
#14143 = CIRCLE ( 'NONE', #2650, 12.00000000000000000 ) ;
#14144 = CARTESIAN_POINT ( 'NONE',  ( -6.500000000000000000, 0.000000000000000000, -3.700000000000000178 ) ) ;
#14145 = ORIENTED_EDGE ( 'NONE', *, *, #13048, .F. ) ;
#14146 = CARTESIAN_POINT ( 'NONE',  ( 4.000000000000000888, -1.656854249492379694, -2.262499999999998401 ) ) ;
#14147 = CARTESIAN_POINT ( 'NONE',  ( 58.03125000000000711, 11.24264068711929276, 18.00000000000000000 ) ) ;
#14148 = CARTESIAN_POINT ( 'NONE',  ( -4.000000000000000000, -1.656854249492383024, 0.4875000027311864881 ) ) ;
#14149 = DIRECTION ( 'NONE',  ( -1.224646799147353207E-16, 0.000000000000000000, -1.000000000000000000 ) ) ;
#14150 = AXIS2_PLACEMENT_3D ( 'NONE', #23618, #12862, #23 ) ;
#14151 = ORIENTED_EDGE ( 'NONE', *, *, #11629, .T. ) ;
#14153 = DIRECTION ( 'NONE',  ( -0.000000000000000000, 0.000000000000000000, -1.000000000000000000 ) ) ;
#14152 = PRESENTATION_LAYER_ASSIGNMENT (  '', '', ( #1876 ) ) ;
#14154 = CARTESIAN_POINT ( 'NONE',  ( -1.432654583217640276, 3.458734125000000326, -3.449999998634403653 ) ) ;
#14155 = CARTESIAN_POINT ( 'NONE',  ( 1.506022603841296714, 0.000000000000000000, 0.000000000000000000 ) ) ;
#14156 = VECTOR ( 'NONE', #5336, 1000.000000000000000 ) ;
#14157 = ORIENTED_EDGE ( 'NONE', *, *, #1429, .F. ) ;
#14158 = DIRECTION ( 'NONE',  ( -1.000000000000000000, -0.000000000000000000, 0.000000000000000000 ) ) ;
#14159 = ORIENTED_EDGE ( 'NONE', *, *, #9138, .F. ) ;
#14160 = FACE_OUTER_BOUND ( 'NONE', #15194, .T. ) ;
#14161 = ORIENTED_EDGE ( 'NONE', *, *, #15533, .T. ) ;
#14162 = CARTESIAN_POINT ( 'NONE',  ( 1.025207404391860050E-15, 3.458734125000000770, 14.43750000136560452 ) ) ;
#14163 = AXIS2_PLACEMENT_3D ( 'NONE', #16505, #83, #7416 ) ;
#14164 = LINE ( 'NONE', #18208, #13046 ) ;
#14165 = AXIS2_PLACEMENT_3D ( 'NONE', #12085, #19349, #10415 ) ;
#14166 = DIRECTION ( 'NONE',  ( 0.000000000000000000, 0.000000000000000000, -1.000000000000000000 ) ) ;
#14167 = CARTESIAN_POINT ( 'NONE',  ( 4.999999999999999112, -4.057423117305329896, -8.475820894093020641 ) ) ;
#14168 = LINE ( 'NONE', #14286, #16719 ) ;
#14169 = CARTESIAN_POINT ( 'NONE',  ( -70.14999999999999147, 8.964466094067258695, 17.50000000000000355 ) ) ;
#14170 = VECTOR ( 'NONE', #2337, 1000.000000000000000 ) ;
#14171 = FACE_OUTER_BOUND ( 'NONE', #10336, .T. ) ;
#14172 = CARTESIAN_POINT ( 'NONE',  ( 60.00000000000000000, 11.54527125603259030, 17.88342085427740713 ) ) ;
#14173 = EDGE_CURVE ( 'NONE', #12637, #4626, #14873, .T. ) ;
#14174 = CARTESIAN_POINT ( 'NONE',  ( -3.458734125000000770, 1.432654583217640498, -2.074999998634404097 ) ) ;
#14175 = CARTESIAN_POINT ( 'NONE',  ( 4.999999999999999112, -4.472189673936728838, -8.264486777890155622 ) ) ;
#14176 = CARTESIAN_POINT ( 'NONE',  ( -2.247776618166700491, 3.308700692843503877, 10.00000000000000888 ) ) ;
#14177 = CARTESIAN_POINT ( 'NONE',  ( -2.445694354108819191, 2.445694354108820523, 16.31250000136560629 ) ) ;
#14178 = LINE ( 'NONE', #12385, #13428 ) ;
#14179 = AXIS2_PLACEMENT_3D ( 'NONE', #5600, #10553, #17827 ) ;
#14180 = ORIENTED_EDGE ( 'NONE', *, *, #17253, .T. ) ;
#14181 = CARTESIAN_POINT ( 'NONE',  ( -71.45000000109247651, 7.933012699999995476, 14.99999999999999645 ) ) ;
#14182 = ORIENTED_EDGE ( 'NONE', *, *, #16513, .T. ) ;
#14183 = CARTESIAN_POINT ( 'NONE',  ( 60.43518183416157541, 9.931948859054379852, 18.99999999999999289 ) ) ;
#14184 = CARTESIAN_POINT ( 'NONE',  ( -66.80000000109247082, 9.143825827087050939, 12.93301269999999370 ) ) ;
#14185 = DIRECTION ( 'NONE',  ( 1.118373553621254909E-32, 0.9073324201775117004, -0.4204139380358592470 ) ) ;
#14186 = ADVANCED_FACE ( 'NONE', ( #8215 ), #22568, .T. ) ;
#14187 = DIRECTION ( 'NONE',  ( -1.000000000000000000, -0.000000000000000000, 0.000000000000000000 ) ) ;
#14188 = ORIENTED_EDGE ( 'NONE', *, *, #11460, .F. ) ;
#14189 = VECTOR ( 'NONE', #19986, 1000.000000000000000 ) ;
#14190 = DIRECTION ( 'NONE',  ( 0.000000000000000000, -0.9510565162951565288, 0.3090169943749382364 ) ) ;
#14191 = VECTOR ( 'NONE', #19412, 1000.000000000000114 ) ;
#14192 = EDGE_LOOP ( 'NONE', ( #5151, #5445, #6684, #21146, #22183, #12890 ) ) ;
#14193 = CYLINDRICAL_SURFACE ( 'NONE', #14498, 2.500000000000002220 ) ;
#14194 = ORIENTED_EDGE ( 'NONE', *, *, #11628, .F. ) ;
#14195 = CARTESIAN_POINT ( 'NONE',  ( 58.43981816583843170, 10.06805114094563791, 17.99999999999999645 ) ) ;
#14196 = CARTESIAN_POINT ( 'NONE',  ( -67.00000000218494733, 9.999999999999998224, 17.49999999999999645 ) ) ;
#14197 = FACE_OUTER_BOUND ( 'NONE', #8036, .T. ) ;
#14198 = CARTESIAN_POINT ( 'NONE',  ( -71.75000000109247367, 8.538419263543524096, 13.53841926354352054 ) ) ;
#14199 = CARTESIAN_POINT ( 'NONE',  ( 3.458734125000002546, -1.432654583217639610, 14.12500000136560452 ) ) ;
#14200 = LINE ( 'NONE', #7245, #6135 ) ;
#14201 = CARTESIAN_POINT ( 'NONE',  ( 58.78125000000000711, 8.757359312880703683, 11.99999999999999822 ) ) ;
#14202 = VECTOR ( 'NONE', #23511, 1000.000000000000000 ) ;
#14203 = CARTESIAN_POINT ( 'NONE',  ( -3.381512639161500466, 0.7267833367865139671, -3.295601554149589330 ) ) ;
#14204 = EDGE_CURVE ( 'NONE', #22615, #11403, #5271, .T. ) ;
#14205 = CARTESIAN_POINT ( 'NONE',  ( 59.81250000000000711, 13.00000000000000000, 14.99999999999998757 ) ) ;
#14206 = EDGE_CURVE ( 'NONE', #16922, #10607, #5094, .T. ) ;
#14207 = CARTESIAN_POINT ( 'NONE',  ( -1.432654583217640498, 3.458734125000000770, 1.800000001365597235 ) ) ;
#14208 = CARTESIAN_POINT ( 'NONE',  ( 67.40000000218495302, 9.999999999999998224, 12.49999999999999289 ) ) ;
#14209 = DIRECTION ( 'NONE',  ( -1.734723475976805517E-15, 0.000000000000000000, 1.000000000000000000 ) ) ;
#14210 = VERTEX_POINT ( 'NONE', #20373 ) ;
#14211 = DIRECTION ( 'NONE',  ( -1.000000000000000000, 0.000000000000000000, 0.000000000000000000 ) ) ;
#14212 = CARTESIAN_POINT ( 'NONE',  ( -35.00000000000000711, 4.500000000000003553, -49.99999999999999289 ) ) ;
#14213 = ORIENTED_EDGE ( 'NONE', *, *, #17260, .T. ) ;
#14214 = CARTESIAN_POINT ( 'NONE',  ( 57.46875000000000711, 6.999999999999992895, 13.75735931288071967 ) ) ;
#14215 =( NAMED_UNIT ( * ) PLANE_ANGLE_UNIT ( ) SI_UNIT ( $, .RADIAN. ) );
#14216 = CARTESIAN_POINT ( 'NONE',  ( 2.828427124746190735, -2.828427124746189847, -0.1999999972688119854 ) ) ;
#14217 = EDGE_CURVE ( 'NONE', #19804, #23527, #8349, .T. ) ;
#14218 = LINE ( 'NONE', #5085, #11311 ) ;
#14219 = ORIENTED_EDGE ( 'NONE', *, *, #20777, .T. ) ;
#14220 = ADVANCED_FACE ( 'NONE', ( #14160 ), #16306, .T. ) ;
#14221 = ORIENTED_EDGE ( 'NONE', *, *, #784, .F. ) ;
#14222 = FACE_OUTER_BOUND ( 'NONE', #458, .T. ) ;
#14223 = CYLINDRICAL_SURFACE ( 'NONE', #15645, 2.500000000000002220 ) ;
#14224 = EDGE_LOOP ( 'NONE', ( #15315, #13253, #13358, #16798 ) ) ;
#14225 = CARTESIAN_POINT ( 'NONE',  ( 42.38741763033275589, -11.25000000000000355, 10.00000000000008882 ) ) ;
#14226 = AXIS2_PLACEMENT_3D ( 'NONE', #22469, #20902, #2714 ) ;
#14227 = CARTESIAN_POINT ( 'NONE',  ( 9.920644283265380691E-16, 4.000000000000000000, 10.75000000000001066 ) ) ;
#14228 = ORIENTED_EDGE ( 'NONE', *, *, #4996, .F. ) ;
#14229 = CARTESIAN_POINT ( 'NONE',  ( 66.65000000109247935, 7.933012699999995476, 14.99999999999999645 ) ) ;
#14230 = CARTESIAN_POINT ( 'NONE',  ( 71.29999999999998295, 9.999999999999998224, 12.49999999999999289 ) ) ;
#14231 = ADVANCED_FACE ( 'NONE', ( #7331 ), #14636, .F. ) ;
#14232 = CARTESIAN_POINT ( 'NONE',  ( 27.50000000000000000, 4.500000000000001776, -31.01025403784447221 ) ) ;
#14233 = LINE ( 'NONE', #16140, #15693 ) ;
#14234 = CARTESIAN_POINT ( 'NONE',  ( 56.09606816583844591, 11.58880310854672935, 10.97181229448534445 ) ) ;
#14235 = EDGE_CURVE ( 'NONE', #14480, #8531, #18087, .T. ) ;
#14236 = CARTESIAN_POINT ( 'NONE',  ( -3.458734125000000326, 0.000000000000000000, 2.737500001365597235 ) ) ;
#14237 = FACE_OUTER_BOUND ( 'NONE', #11116, .T. ) ;
#14238 = CARTESIAN_POINT ( 'NONE',  ( -2.445694354108818303, -2.445694354108820523, 16.56250000136560629 ) ) ;
#14239 = CARTESIAN_POINT ( 'NONE',  ( 4.000000000000000000, 1.656854249492381248, -0.1374999999999984290 ) ) ;
#14240 = ORIENTED_EDGE ( 'NONE', *, *, #23411, .F. ) ;
#14241 = CARTESIAN_POINT ( 'NONE',  ( 0.000000000000000000, -8.734705317681630277, 0.4999240074894146790 ) ) ;
#14242 = DIRECTION ( 'NONE',  ( 0.000000000000000000, 0.000000000000000000, -1.000000000000000000 ) ) ;
#14243 = DIRECTION ( 'NONE',  ( 0.3420201433256622736, -0.9396926207859106484, -1.232595164407828100E-31 ) ) ;
#14244 = EDGE_CURVE ( 'NONE', #20275, #3528, #7972, .T. ) ;
#14245 = EDGE_CURVE ( 'NONE', #10661, #17331, #7207, .T. ) ;
#14246 = ORIENTED_EDGE ( 'NONE', *, *, #4401, .T. ) ;
#14247 = CARTESIAN_POINT ( 'NONE',  ( 4.999999999999999112, 1.239665997527020558, -9.314797388894877628 ) ) ;
#14248 = LINE ( 'NONE', #1386, #6860 ) ;
#14249 = CARTESIAN_POINT ( 'NONE',  ( -2.000000000000001776, 0.000000000000000000, 0.000000000000000000 ) ) ;
#14250 = ORIENTED_EDGE ( 'NONE', *, *, #18614, .T. ) ;
#14251 = CARTESIAN_POINT ( 'NONE',  ( -69.39999999999999147, 8.232233047033627571, 16.76776695296636532 ) ) ;
#14252 = ORIENTED_EDGE ( 'NONE', *, *, #1901, .T. ) ;
#14253 = B_SPLINE_CURVE_WITH_KNOTS ( 'NONE', 3,
 ( #14343, #18147, #10641, #6909, #8840, #5214, #3423, #9070 ),
 .UNSPECIFIED., .F., .F.,
 ( 4, 2, 2, 4 ),
 ( 0.005725059856848645212, 0.006314084072593634418, 0.006903108288338624492, 0.008081156719828603771 ),
 .UNSPECIFIED. ) ;
#14254 = CARTESIAN_POINT ( 'NONE',  ( 53.06250000000000711, 5.999999999999996447, 15.00000000000001599 ) ) ;
#14255 = CARTESIAN_POINT ( 'NONE',  ( 66.70000000218495018, 11.76776695296636888, 13.23223304703362579 ) ) ;
#14256 = FACE_OUTER_BOUND ( 'NONE', #21661, .T. ) ;
#14257 = DIRECTION ( 'NONE',  ( -1.000000000000000000, -0.000000000000000000, -0.000000000000000000 ) ) ;
#14258 = CARTESIAN_POINT ( 'NONE',  ( 65.85000000109246798, 9.999999999999998224, 17.06698730000000097 ) ) ;
#14259 = ORIENTED_EDGE ( 'NONE', *, *, #7202, .T. ) ;
#14260 = CARTESIAN_POINT ( 'NONE',  ( -3.999999999999999112, 1.656854249492380582, 10.06250000273119660 ) ) ;
#14261 = CARTESIAN_POINT ( 'NONE',  ( 52.18518183416157541, 10.06805114094562548, 11.99999999999999645 ) ) ;
#14262 = DIRECTION ( 'NONE',  ( 0.000000000000000000, 1.000000000000000000, 0.000000000000000000 ) ) ;
#14263 = CARTESIAN_POINT ( 'NONE',  ( 67.75000000109245946, 8.538419263543524096, 13.53841926354352054 ) ) ;
#14264 = CARTESIAN_POINT ( 'NONE',  ( -3.458734124999998993, -1.432654583217642497, 17.75000000136560629 ) ) ;
#14265 = CARTESIAN_POINT ( 'NONE',  ( 0.000000000000000000, 6.772677083992387992, 5.538577986808924436 ) ) ;
#14266 = DIRECTION ( 'NONE',  ( 0.8660254037844381525, -0.5000000000000006661, 0.000000000000000000 ) ) ;
#14267 = ORIENTED_EDGE ( 'NONE', *, *, #1202, .T. ) ;
#14268 = DIRECTION ( 'NONE',  ( 1.000000000000000000, -0.000000000000000000, -0.000000000000000000 ) ) ;
#14269 = CARTESIAN_POINT ( 'NONE',  ( 57.28125000000000711, 8.757359312880703683, 11.99999999999999822 ) ) ;
#14270 = CARTESIAN_POINT ( 'NONE',  ( -2.828427124746189403, 2.828427124746190291, 11.00000000273119660 ) ) ;
#14271 = ADVANCED_FACE ( 'NONE', ( #1420, #19873 ), #5039, .F. ) ;
#14272 = EDGE_CURVE ( 'NONE', #22281, #12677, #8327, .T. ) ;
#14273 = ORIENTED_EDGE ( 'NONE', *, *, #9384, .T. ) ;
#14274 = PLANE ( 'NONE',  #7489 ) ;
#14275 = CARTESIAN_POINT ( 'NONE',  ( -1.432654583217640942, -3.458734124999999882, -1.074999998634403209 ) ) ;
#14276 = CARTESIAN_POINT ( 'NONE',  ( 0.000000000000000000, 2.223716399045570835, 8.461683424509324425 ) ) ;
#14277 = VERTEX_POINT ( 'NONE', #8762 ) ;
#14278 = CARTESIAN_POINT ( 'NONE',  ( -4.000000000000004441, 2.309401076758496263, -3.504269196027523847 ) ) ;
#14279 = ORIENTED_EDGE ( 'NONE', *, *, #18463, .T. ) ;
#14280 = LINE ( 'NONE', #23593, #14471 ) ;
#14281 = ORIENTED_EDGE ( 'NONE', *, *, #15214, .T. ) ;
#14282 = CARTESIAN_POINT ( 'NONE',  ( -1.656854249492379250, 4.000000000000000000, 19.81250000000001776 ) ) ;
#14283 = CARTESIAN_POINT ( 'NONE',  ( 0.000000000000000000, 0.000000000000000000, 0.000000000000000000 ) ) ;
#14284 = PLANE ( 'NONE',  #737 ) ;
#14285 = CIRCLE ( 'NONE', #3927, 9.000000000000000000 ) ;
#14286 = CARTESIAN_POINT ( 'NONE',  ( 42.38741763033275589, -11.25000000000000355, 5.000000000000079936 ) ) ;
#14287 = CARTESIAN_POINT ( 'NONE',  ( -70.54999999999999716, 11.03553390593273598, 12.49999999999999289 ) ) ;
#14288 = VECTOR ( 'NONE', #17048, 1000.000000000000000 ) ;
#14289 = LINE ( 'NONE', #14410, #9161 ) ;
#14290 = CARTESIAN_POINT ( 'NONE',  ( 60.00000000000000000, 12.03166802832783766, 18.18714555911078889 ) ) ;
#14291 = CARTESIAN_POINT ( 'NONE',  ( -2.445694354108819635, -2.445694354108820967, 1.112500001365595681 ) ) ;
#14292 = CARTESIAN_POINT ( 'NONE',  ( 67.35000000218495586, 8.964466094067256918, 12.49999999999999822 ) ) ;
#14293 = CARTESIAN_POINT ( 'NONE',  ( 68.09999999999999432, 9.999999999999998224, 12.49999999999999289 ) ) ;
#14294 = CARTESIAN_POINT ( 'NONE',  ( -1.432654583217639610, -3.458734124999999882, 17.62500000136560274 ) ) ;
#14295 = FACE_OUTER_BOUND ( 'NONE', #14834, .T. ) ;
#14296 = ORIENTED_EDGE ( 'NONE', *, *, #10631, .T. ) ;
#14297 = FACE_OUTER_BOUND ( 'NONE', #8057, .T. ) ;
#14298 = VERTEX_POINT ( 'NONE', #16068 ) ;
#14299 = CARTESIAN_POINT ( 'NONE',  ( 55.65393183416158251, 5.971812294485358663, 16.58880310854675599 ) ) ;
#14300 = CARTESIAN_POINT ( 'NONE',  ( -68.80000000109247082, 10.85617417291294551, 17.06698729999999742 ) ) ;
#14301 =( NAMED_UNIT ( * ) PLANE_ANGLE_UNIT ( ) SI_UNIT ( $, .RADIAN. ) );
#14302 = DIRECTION ( 'NONE',  ( -1.000000000000000000, -0.000000000000000000, -0.000000000000000000 ) ) ;
#14303 = ORIENTED_EDGE ( 'NONE', *, *, #22526, .F. ) ;
#14304 = DIRECTION ( 'NONE',  ( -1.000000000000000000, 0.000000000000000000, 0.000000000000000000 ) ) ;
#14305 = AXIS2_PLACEMENT_3D ( 'NONE', #5257, #96, #16292 ) ;
#14306 = PRODUCT_RELATED_PRODUCT_CATEGORY ( 'part', '', ( #13562 ) ) ;
#14307 = VERTEX_POINT ( 'NONE', #23358 ) ;
#14308 = CARTESIAN_POINT ( 'NONE',  ( -71.92500000163870766, 9.999999999999998224, 17.28349365000000049 ) ) ;
#14309 = ORIENTED_EDGE ( 'NONE', *, *, #3762, .T. ) ;
#14310 = CARTESIAN_POINT ( 'NONE',  ( 53.75231816583844591, 7.926799079670502124, 17.16943976678978245 ) ) ;
#14311 = EDGE_CURVE ( 'NONE', #21477, #11647, #1669, .T. ) ;
#14312 = CARTESIAN_POINT ( 'NONE',  ( -67.20000000218495018, 7.499999999999996447, 14.99999999999999645 ) ) ;
#14313 = DIRECTION ( 'NONE',  ( -1.000000000000000000, -0.000000000000000000, 0.000000000000000000 ) ) ;
#14314 = CLOSED_SHELL ( 'NONE', ( #18891, #20710, #4100, #7827, #17108, #2630, #13586, #282, #1865, #11317, #12879, #721, #14842, #10334, #11901, #1863, #5432, #13280, #20234, #14774, #852, #2762, #5155, #19054, #21694, #5006, #11762, #12479, #21852, #12152, #7475, #7277 ) ) ;
#14315 = DIRECTION ( 'NONE',  ( 7.087422195345011518E-32, 1.000000000000000000, -0.000000000000000000 ) ) ;
#14316 = CARTESIAN_POINT ( 'NONE',  ( 1.872352939448454495E-15, -3.458734125000000770, 16.93750000136560629 ) ) ;
#14317 = CARTESIAN_POINT ( 'NONE',  ( 4.999999999999999112, 7.360373001730920350, 4.729683950898897926 ) ) ;
#14318 = CARTESIAN_POINT ( 'NONE',  ( 55.87500000000000711, 7.878679656440349177, 12.87867965644035984 ) ) ;
#14319 = CARTESIAN_POINT ( 'NONE',  ( 66.94999999999998863, 8.964466094067207180, 17.49999999999995026 ) ) ;
#14320 = CARTESIAN_POINT ( 'NONE',  ( 56.53125000000000711, 11.24264068711929276, 18.00000000000000355 ) ) ;
#14321 = CARTESIAN_POINT ( 'NONE',  ( -3.458734125000000770, 1.432654583217640498, -2.074999998634404097 ) ) ;
#14322 = DIRECTION ( 'NONE',  ( 0.000000000000000000, 0.000000000000000000, -1.000000000000000000 ) ) ;
#14323 = CARTESIAN_POINT ( 'NONE',  ( -68.45000000000000284, 11.03553390593276617, 17.49999999999997513 ) ) ;
#14324 = ORIENTED_EDGE ( 'NONE', *, *, #9861, .T. ) ;
#14325 = CARTESIAN_POINT ( 'NONE',  ( 2.500000000000000888, 3.061616997868384127E-16, -4.974599999999998801 ) ) ;
#14326 = CARTESIAN_POINT ( 'NONE',  ( -1.287237434361707233, -3.875615274277397937, -3.430618716626816500 ) ) ;
#14327 = ORIENTED_EDGE ( 'NONE', *, *, #8220, .T. ) ;
#14328 = DIRECTION ( 'NONE',  ( 2.465190328815655597E-32, 0.3420201433256690460, -0.9396926207859082059 ) ) ;
#14329 = CARTESIAN_POINT ( 'NONE',  ( 1.656854249492380360, 4.000000000000000000, 1.112500002731187099 ) ) ;
#14330 = CARTESIAN_POINT ( 'NONE',  ( -14.98018309676619175, -9.000000000000003553, 5.000000000000079936 ) ) ;
#14331 = VERTEX_POINT ( 'NONE', #23225 ) ;
#14332 = CARTESIAN_POINT ( 'NONE',  ( 1.656854249492384135, -3.999999999999999112, 16.31250000000001066 ) ) ;
#14333 = ORIENTED_EDGE ( 'NONE', *, *, #21731, .F. ) ;
#14334 = PLANE ( 'NONE',  #12557 ) ;
#14335 = AXIS2_PLACEMENT_3D ( 'NONE', #23305, #10413, #12434 ) ;
#14336 = PLANE ( 'NONE',  #16770 ) ;
#14337 = ORIENTED_EDGE ( 'NONE', *, *, #13845, .T. ) ;
#14338 = DIRECTION ( 'NONE',  ( -1.000000000000000000, -0.000000000000000000, -0.000000000000000000 ) ) ;
#14339 = B_SPLINE_CURVE_WITH_KNOTS ( 'NONE', 3,
 ( #8104, #530, #11817, #15528, #5602, #22676, #15176, #20191 ),
 .UNSPECIFIED., .F., .F.,
 ( 4, 2, 2, 4 ),
 ( 0.003797433802554453681, 0.004743183970586248299, 0.005688934138618042917, 0.007580434474681630418 ),
 .UNSPECIFIED. ) ;
#14340 = EDGE_CURVE ( 'NONE', #6517, #4629, #14280, .T. ) ;
#14341 = CARTESIAN_POINT ( 'NONE',  ( 4.000000000000000888, 4.898587196589412829E-16, 11.50000000000001066 ) ) ;
#14342 = EDGE_CURVE ( 'NONE', #11449, #17388, #5150, .T. ) ;
#14343 = CARTESIAN_POINT ( 'NONE',  ( 4.000000000000000000, 0.000000000000000000, 0.000000000000000000 ) ) ;
#14344 = CARTESIAN_POINT ( 'NONE',  ( 66.10000000109246798, 7.933012699999995476, 14.14382582708705094 ) ) ;
#14345 = AXIS2_PLACEMENT_3D ( 'NONE', #22350, #13289, #23306 ) ;
#14346 = EDGE_CURVE ( 'NONE', #10762, #839, #18111, .T. ) ;
#14347 = CARTESIAN_POINT ( 'NONE',  ( 0.000000000000000000, 0.000000000000000000, -3.700000000000000178 ) ) ;
#14349 = DIRECTION ( 'NONE',  ( 7.087422195345011518E-32, 1.000000000000000000, -0.000000000000000000 ) ) ;
#14348 = AXIS2_PLACEMENT_3D ( 'NONE', #9404, #16578, #5438 ) ;
#14350 = CARTESIAN_POINT ( 'NONE',  ( 52.21875000000002842, 14.00000000000000888, 16.65685424949235482 ) ) ;
#14351 = AXIS2_PLACEMENT_3D ( 'NONE', #19158, #15475, #831 ) ;
#14352 = CARTESIAN_POINT ( 'NONE',  ( 3.458734125000000770, -1.432654583217639610, 3.175000001365598568 ) ) ;
#14353 = CARTESIAN_POINT ( 'NONE',  ( 3.458734125000002102, -1.432654583217639610, 15.87500000136560452 ) ) ;
#14354 = CARTESIAN_POINT ( 'NONE',  ( 1.656854249492384135, -3.999999999999999112, 18.43750000273119483 ) ) ;
#14355 = CARTESIAN_POINT ( 'NONE',  ( -70.45000000218495018, 7.499999999999996447, 13.96446609406725514 ) ) ;
#14356 = ORIENTED_EDGE ( 'NONE', *, *, #9366, .T. ) ;
#14357 = DIRECTION ( 'NONE',  ( 0.000000000000000000, -1.000000000000000000, 0.000000000000000000 ) ) ;
#14358 = CARTESIAN_POINT ( 'NONE',  ( 68.45000000000000284, 11.03553390593276617, 17.49999999999997513 ) ) ;
#14359 = CARTESIAN_POINT ( 'NONE',  ( 4.999999999999999112, 10.82112760146739205, -1.975651141462126059 ) ) ;
#14360 = ORIENTED_EDGE ( 'NONE', *, *, #21487, .T. ) ;
#14361 = DIRECTION ( 'NONE',  ( -1.000000000000000000, 0.000000000000000000, -0.000000000000000000 ) ) ;
#14362 = EDGE_CURVE ( 'NONE', #12919, #8667, #5656, .T. ) ;
#14363 = VERTEX_POINT ( 'NONE', #9128 ) ;
#14364 = CARTESIAN_POINT ( 'NONE',  ( 71.10000000218494165, 8.232233047033627571, 16.76776695296636532 ) ) ;
#14365 = ORIENTED_EDGE ( 'NONE', *, *, #20736, .F. ) ;
#14366 = CARTESIAN_POINT ( 'NONE',  ( 65.85000000218495586, 11.03553390593269867, 12.49999999999995559 ) ) ;
#14367 = ORIENTED_EDGE ( 'NONE', *, *, #18879, .F. ) ;
#14368 = AXIS2_PLACEMENT_3D ( 'NONE', #18200, #2253, #18541 ) ;
#14369 = CARTESIAN_POINT ( 'NONE',  ( 54.84375000000000000, 8.343145750507638070, 19.00000000000000711 ) ) ;
#14370 = AXIS2_PLACEMENT_3D ( 'NONE', #10689, #17963, #10214 ) ;
#14371 = EDGE_CURVE ( 'NONE', #10183, #21260, #7221, .T. ) ;
#14372 = VECTOR ( 'NONE', #8492, 1000.000000000000000 ) ;
#14373 = CARTESIAN_POINT ( 'NONE',  ( 67.75000000218496155, 11.03553390593273598, 17.50000000000000355 ) ) ;
#14374 = DIRECTION ( 'NONE',  ( 1.000000000000000000, 0.000000000000000000, 0.000000000000000000 ) ) ;
#14375 = CARTESIAN_POINT ( 'NONE',  ( -19.99999999999999645, -9.000000000000003553, 10.00000000000008882 ) ) ;
#14376 = CARTESIAN_POINT ( 'NONE',  ( 2.499999999999999556, -9.680994141368808314, 5.222868219166821646 ) ) ;
#14377 = EDGE_CURVE ( 'NONE', #6003, #9988, #20943, .T. ) ;
#14378 = ORIENTED_EDGE ( 'NONE', *, *, #17482, .T. ) ;
#14379 = EDGE_CURVE ( 'NONE', #14967, #21785, #470, .T. ) ;
#14380 = CARTESIAN_POINT ( 'NONE',  ( 0.000000000000000000, -2.223716399045513548, -8.461683424509336859 ) ) ;
#14381 = CARTESIAN_POINT ( 'NONE',  ( 57.24768183416158962, 7.123453452023678523, 17.78030770151605822 ) ) ;
#14382 = CARTESIAN_POINT ( 'NONE',  ( -4.714285714285714413, 5.773334910266094008E-16, 3.059999999999998277 ) ) ;
#14383 = PLANE ( 'NONE',  #22525 ) ;
#14384 = DIRECTION ( 'NONE',  ( 0.9396926207859107594, -0.3420201433256623291, 3.697785493223492838E-32 ) ) ;
#14385 = ORIENTED_EDGE ( 'NONE', *, *, #10989, .F. ) ;
#14386 = DIRECTION ( 'NONE',  ( 0.000000000000000000, -1.000000000000000000, 0.000000000000000000 ) ) ;
#14387 = CARTESIAN_POINT ( 'NONE',  ( 55.96875000000001421, 6.999999999999992006, 13.75735931288071967 ) ) ;
#14388 = VECTOR ( 'NONE', #17811, 1000.000000000000000 ) ;
#14389 = DIRECTION ( 'NONE',  ( 0.000000000000000000, 0.000000000000000000, -1.000000000000000000 ) ) ;
#14390 = ORIENTED_EDGE ( 'NONE', *, *, #13970, .T. ) ;
#14391 = DIRECTION ( 'NONE',  ( 1.000000000000000000, 0.000000000000000000, -1.224646799147353207E-16 ) ) ;
#14392 = CARTESIAN_POINT ( 'NONE',  ( 3.458734125000000326, 4.235727675282971730E-16, -2.762499998634404097 ) ) ;
#14393 = LINE ( 'NONE', #1547, #20045 ) ;
#14394 = ORIENTED_EDGE ( 'NONE', *, *, #5899, .F. ) ;
#14395 = FACE_BOUND ( 'NONE', #12976, .T. ) ;
#14396 = ORIENTED_EDGE ( 'NONE', *, *, #23602, .T. ) ;
#14397 = AXIS2_PLACEMENT_3D ( 'NONE', #20692, #8259, #8024 ) ;
#14398 = AXIS2_PLACEMENT_3D ( 'NONE', #19040, #13915, #8284 ) ;
#14399 = CARTESIAN_POINT ( 'NONE',  ( -1.656854249492379472, 4.000000000000000000, 18.81250000000001421 ) ) ;
#14400 = CARTESIAN_POINT ( 'NONE',  ( -1.656854249492379250, 4.000000000000000000, 18.81250000000001776 ) ) ;
#14401 = LINE ( 'NONE', #8892, #12682 ) ;
#14402 = AXIS2_PLACEMENT_3D ( 'NONE', #6719, #21293, #4916 ) ;
#14403 = CARTESIAN_POINT ( 'NONE',  ( 47.85166990323382663, -9.000000000000003553, 5.000000000000079936 ) ) ;
#14404 = EDGE_CURVE ( 'NONE', #21785, #12149, #11038, .T. ) ;
#14405 = DIRECTION ( 'NONE',  ( 0.000000000000000000, 0.000000000000000000, -1.000000000000000000 ) ) ;
#14406 = EDGE_CURVE ( 'NONE', #5525, #19779, #1905, .T. ) ;
#14407 = CYLINDRICAL_SURFACE ( 'NONE', #20899, 9.000000000000000000 ) ;
#14408 = EDGE_CURVE ( 'NONE', #13238, #7010, #20540, .T. ) ;
#14409 = CARTESIAN_POINT ( 'NONE',  ( -67.74999999999998579, 8.964466094067258695, 17.50000000000000355 ) ) ;
#14410 = CARTESIAN_POINT ( 'NONE',  ( 22.10407284676620066, -9.000000000000003553, 5.000000000000079936 ) ) ;
#14411 = CARTESIAN_POINT ( 'NONE',  ( 59.99999999999995026, 12.29613458025714401, 18.03534775876610752 ) ) ;
#14412 = DIRECTION ( 'NONE',  ( 0.000000000000000000, 0.000000000000000000, -1.000000000000000000 ) ) ;
#14413 = CARTESIAN_POINT ( 'NONE',  ( 1.656854249492380360, 4.000000000000000000, 3.987500000000003375 ) ) ;
#14414 = CARTESIAN_POINT ( 'NONE',  ( -66.15000000109247935, 8.538419263543524096, 13.53841926354352054 ) ) ;
#14415 = CARTESIAN_POINT ( 'NONE',  ( 4.999999999999999112, 5.538577986808900455, 6.772677083992405755 ) ) ;
#14416 = CARTESIAN_POINT ( 'NONE',  ( 1.432654583217641164, 3.458734125000000326, 17.12500000136560629 ) ) ;
#14417 = DIRECTION ( 'NONE',  ( 0.000000000000000000, 0.000000000000000000, 1.000000000000000000 ) ) ;
#14418 = ORIENTED_EDGE ( 'NONE', *, *, #14244, .F. ) ;
#14419 = CARTESIAN_POINT ( 'NONE',  ( -71.30000000109249925, 9.143825827087049163, 17.06698730000000097 ) ) ;
#14420 = VERTEX_POINT ( 'NONE', #14754 ) ;
#14421 = CARTESIAN_POINT ( 'NONE',  ( 53.49768183416157541, 12.87654654797631792, 12.21969229848393113 ) ) ;
#14422 = CARTESIAN_POINT ( 'NONE',  ( -66.70000000109246230, 7.933012699999995476, 14.14382582708705094 ) ) ;
#14423 = DIRECTION ( 'NONE',  ( -1.000000000000000000, 0.000000000000000000, 0.000000000000000000 ) ) ;
#14424 = CARTESIAN_POINT ( 'NONE',  ( -3.381512639161500466, 0.7267833367865139671, -3.295601554149589330 ) ) ;
#14425 = ORIENTED_EDGE ( 'NONE', *, *, #21928, .T. ) ;
#14426 = FACE_OUTER_BOUND ( 'NONE', #8765, .T. ) ;
#14427 = VERTEX_POINT ( 'NONE', #9248 ) ;
#14428 = CARTESIAN_POINT ( 'NONE',  ( 71.00000000000000000, 8.232233047033627571, 16.76776695296636532 ) ) ;
#14429 = ORIENTED_EDGE ( 'NONE', *, *, #19440, .T. ) ;
#14430 = CARTESIAN_POINT ( 'NONE',  ( 59.25000000000000711, 7.878679656440361612, 17.12132034355964549 ) ) ;
#14431 = CARTESIAN_POINT ( 'NONE',  ( -71.85000000109246798, 12.06698730000000097, 14.99999999999999645 ) ) ;
#14432 = CARTESIAN_POINT ( 'NONE',  ( -70.45000000109247651, 12.06698730000000097, 14.99999999999999645 ) ) ;
#14433 = CARTESIAN_POINT ( 'NONE',  ( 1.432654583217641386, 3.458734125000000770, 16.37500000136560629 ) ) ;
#14434 = LINE ( 'NONE', #16336, #10741 ) ;
#14435 = CARTESIAN_POINT ( 'NONE',  ( 52.40625000000000000, 12.99999999999999645, 13.75735931288070191 ) ) ;
#14436 = FACE_OUTER_BOUND ( 'NONE', #14848, .T. ) ;
#14437 = CARTESIAN_POINT ( 'NONE',  ( 59.25000000000000711, 7.878679656440361612, 17.12132034355964549 ) ) ;
#14438 = CARTESIAN_POINT ( 'NONE',  ( -19.99999999999999645, -9.000000000000003553, 10.00000000000008882 ) ) ;
#14439 = CARTESIAN_POINT ( 'NONE',  ( -3.999999999999999112, 1.656854249492380804, 18.06250000273119838 ) ) ;
#14440 = DIRECTION ( 'NONE',  ( -1.000000000000000000, 0.000000000000000000, 0.000000000000000000 ) ) ;
#14441 = VECTOR ( 'NONE', #13135, 1000.000000000000000 ) ;
#14442 = EDGE_CURVE ( 'NONE', #14730, #315, #18437, .T. ) ;
#14443 = ORIENTED_EDGE ( 'NONE', *, *, #15013, .F. ) ;
#14444 = DIRECTION ( 'NONE',  ( -1.000000000000000000, 0.000000000000000000, 0.000000000000000000 ) ) ;
#14445 = LINE ( 'NONE', #14212, #22734 ) ;
#14446 = VERTEX_POINT ( 'NONE', #20098 ) ;
#14447 = CARTESIAN_POINT ( 'NONE',  ( 54.65625000000001421, 7.000000000000003553, 16.24264068711929099 ) ) ;
#14448 = CARTESIAN_POINT ( 'NONE',  ( 1.656854249492383024, -3.999999999999999112, 0.7375000027311867656 ) ) ;
#14449 = DIRECTION ( 'NONE',  ( -0.000000000000000000, 1.000000000000000000, -0.000000000000000000 ) ) ;
#14450 = ORIENTED_EDGE ( 'NONE', *, *, #7309, .T. ) ;
#14451 = CARTESIAN_POINT ( 'NONE',  ( -1.656854249492379250, 4.000000000000000000, 16.81250000000001066 ) ) ;
#14452 = VERTEX_POINT ( 'NONE', #107 ) ;
#14453 = VECTOR ( 'NONE', #23234, 1000.000000000000000 ) ;
#14454 = CARTESIAN_POINT ( 'NONE',  ( 66.20000000218495018, 9.999999999999998224, 17.49999999999999645 ) ) ;
#14455 = ORIENTED_EDGE ( 'NONE', *, *, #14953, .F. ) ;
#14456 = FACE_BOUND ( 'NONE', #18203, .T. ) ;
#14457 = VECTOR ( 'NONE', #9771, 1000.000000000000227 ) ;
#14458 = CYLINDRICAL_SURFACE ( 'NONE', #21280, 4.000000000000001776 ) ;
#14459 = ORIENTED_EDGE ( 'NONE', *, *, #14371, .F. ) ;
#14460 = DIRECTION ( 'NONE',  ( -0.3420201433256622181, 0.9396926207859106484, 1.232595164407828100E-31 ) ) ;
#14461 = AXIS2_PLACEMENT_3D ( 'NONE', #1864, #11488, #5708 ) ;
#14462 = VECTOR ( 'NONE', #692, 1000.000000000000000 ) ;
#14463 = CARTESIAN_POINT ( 'NONE',  ( 65.90000000109246514, 9.143825827087049163, 17.06698729999999742 ) ) ;
#14464 = CARTESIAN_POINT ( 'NONE',  ( -65.40000000218495302, 9.999999999999998224, 17.49999999999999645 ) ) ;
#14465 = FACE_OUTER_BOUND ( 'NONE', #16475, .T. ) ;
#14466 = CARTESIAN_POINT ( 'NONE',  ( 57.03356816583845301, 11.72490539043803004, 18.97181229448534268 ) ) ;
#14467 = CARTESIAN_POINT ( 'NONE',  ( -3.458734125000000326, 0.000000000000000000, -0.2624999986344037084 ) ) ;
#14468 = SURFACE_SIDE_STYLE ('',( #12565 ) ) ;
#14469 = CARTESIAN_POINT ( 'NONE',  ( -3.458734124999998993, 0.000000000000000000, 13.43750000136560452 ) ) ;
#14470 = DIRECTION ( 'NONE',  ( 0.000000000000000000, 1.224646799147353454E-16, 1.000000000000000000 ) ) ;
#14471 = VECTOR ( 'NONE', #12492, 1000.000000000000000 ) ;
#14472 = ADVANCED_FACE ( 'NONE', ( #9355 ), #7683, .F. ) ;
#14473 = CARTESIAN_POINT ( 'NONE',  ( 4.999999999999999112, 6.772677083992466152, -5.538577986808826736 ) ) ;
#14474 = ORIENTED_EDGE ( 'NONE', *, *, #3972, .F. ) ;
#14475 = DIRECTION ( 'NONE',  ( -1.000000000000000000, -4.625929269271485914E-16, 1.224646799147353454E-16 ) ) ;
#14476 = DIRECTION ( 'NONE',  ( -1.000000000000000000, -0.000000000000000000, -0.000000000000000000 ) ) ;
#14477 = DIRECTION ( 'NONE',  ( 0.000000000000000000, 0.000000000000000000, -1.000000000000000000 ) ) ;
#14478 = ORIENTED_EDGE ( 'NONE', *, *, #12020, .T. ) ;
#14479 = CIRCLE ( 'NONE', #22472, 2.500000000000002220 ) ;
#14480 = VERTEX_POINT ( 'NONE', #7440 ) ;
#14481 = CIRCLE ( 'NONE', #4519, 8.073750000000021743 ) ;
#14482 = DIRECTION ( 'NONE',  ( 0.000000000000000000, 0.5877852522924743583, -0.8090169943749467851 ) ) ;
#14483 = ORIENTED_EDGE ( 'NONE', *, *, #13786, .T. ) ;
#14484 = EDGE_CURVE ( 'NONE', #11306, #4949, #6646, .T. ) ;
#14485 = CARTESIAN_POINT ( 'NONE',  ( 57.46875000000000711, 5.999999999999987566, 13.34314575050763452 ) ) ;
#14486 = ORIENTED_EDGE ( 'NONE', *, *, #22569, .T. ) ;
#14487 = DIRECTION ( 'NONE',  ( -0.000000000000000000, -1.000000000000000000, 0.000000000000000000 ) ) ;
#14488 = ORIENTED_EDGE ( 'NONE', *, *, #639, .T. ) ;
#14489 = CARTESIAN_POINT ( 'NONE',  ( 52.03124999999999289, 11.65685424949239923, 18.99999999999998934 ) ) ;
#14490 = CARTESIAN_POINT ( 'NONE',  ( 67.15000000218495302, 7.499999999999995559, 16.03553390593273420 ) ) ;
#14491 = VECTOR ( 'NONE', #4536, 1000.000000000000000 ) ;
#14492 = LINE ( 'NONE', #9097, #9193 ) ;
#14493 =( BOUNDED_CURVE ( )  B_SPLINE_CURVE ( 2, ( #18502, #11710, #11228, #4135, #6056, #5938, #13264, #20528, #181 ),
 .UNSPECIFIED., .F., .F. ) 
 B_SPLINE_CURVE_WITH_KNOTS ( ( 3, 2, 2, 2, 3 ),
 ( 0.4374999999999995004, 0.4531249999999993894, 0.4687499999999993339, 0.4843749999999992228, 0.4999999999999991118 ),
 .UNSPECIFIED. ) 
 CURVE ( )  GEOMETRIC_REPRESENTATION_ITEM ( )  RATIONAL_B_SPLINE_CURVE ( ( 1.000000000000002442, 0.9238795325112842960, 1.000000000000000000, 0.9238795325112867385, 1.000000000000000000, 0.9238795325112867385, 1.000000000000000000, 0.9238795325112910684, 0.9999999999999956701 ) ) 
 REPRESENTATION_ITEM ( '' )  );
#14494 = LINE ( 'NONE', #14375, #2200 ) ;
#14495 = CARTESIAN_POINT ( 'NONE',  ( 0.000000000000000000, 7.360373001730986964, -4.729683950898791345 ) ) ;
#14496 = ORIENTED_EDGE ( 'NONE', *, *, #14808, .T. ) ;
#14497 = CARTESIAN_POINT ( 'NONE',  ( 9.920644283265380691E-16, 4.000000000000000000, 10.75000000000001066 ) ) ;
#14498 = AXIS2_PLACEMENT_3D ( 'NONE', #6752, #19203, #8452 ) ;
#14499 = LINE ( 'NONE', #23693, #19469 ) ;
#14500 = CARTESIAN_POINT ( 'NONE',  ( 52.09143183416158251, 11.31069182806491291, 12.02818770551463778 ) ) ;
#14501 = CARTESIAN_POINT ( 'NONE',  ( 3.789206216388694148, -0.2381715126799111015, 2.039999999999999591 ) ) ;
#14502 = CARTESIAN_POINT ( 'NONE',  ( 66.50000000109245946, 12.06698730000000275, 15.85617417291294196 ) ) ;
#14503 = DIRECTION ( 'NONE',  ( -1.000000000000000000, 0.000000000000000000, -0.000000000000000000 ) ) ;
#14504 = EDGE_CURVE ( 'NONE', #10070, #11881, #18672, .T. ) ;
#14505 = DIRECTION ( 'NONE',  ( -1.000000000000000000, 0.000000000000000000, 1.224646799147353207E-16 ) ) ;
#14506 = ORIENTED_EDGE ( 'NONE', *, *, #21493, .T. ) ;
#14507 = FACE_OUTER_BOUND ( 'NONE', #268, .T. ) ;
#14508 = EDGE_CURVE ( 'NONE', #549, #5170, #16646, .T. ) ;
#14509 = CARTESIAN_POINT ( 'NONE',  ( 54.28125000000000000, 8.757359312880703683, 11.99999999999999822 ) ) ;
#14510 = LINE ( 'NONE', #4052, #20388 ) ;
#14511 = CARTESIAN_POINT ( 'NONE',  ( -72.45000000000001705, 11.03553390593273953, 17.50000000000000355 ) ) ;
#14512 = ORIENTED_EDGE ( 'NONE', *, *, #20893, .F. ) ;
#14513 = CIRCLE ( 'NONE', #17559, 8.749000000000002331 ) ;
#14514 = CARTESIAN_POINT ( 'NONE',  ( 34.67968829071656245, -8.974600000000002353, 10.00000000000008882 ) ) ;
#14515 = FACE_OUTER_BOUND ( 'NONE', #15911, .T. ) ;
#14516 = CARTESIAN_POINT ( 'NONE',  ( 2.345747346278113987, -3.264484291692503870, -0.01223254789874484924 ) ) ;
#14517 = ADVANCED_FACE ( 'NONE', ( #7552 ), #5749, .F. ) ;
#14518 = VERTEX_POINT ( 'NONE', #18548 ) ;
#14519 = CARTESIAN_POINT ( 'NONE',  ( 69.70000000000000284, 9.999999999999998224, 12.49999999999999289 ) ) ;
#14520 = VERTEX_POINT ( 'NONE', #2135 ) ;
#14521 = EDGE_CURVE ( 'NONE', #5354, #946, #9469, .T. ) ;
#14522 = CARTESIAN_POINT ( 'NONE',  ( -3.999999999999999112, 0.000000000000000000, 19.00000000000001066 ) ) ;
#14523 = AXIS2_PLACEMENT_3D ( 'NONE', #11751, #2607, #9950 ) ;
#14524 = CARTESIAN_POINT ( 'NONE',  ( -3.458734124999999437, 1.432654583217640498, 10.62500000136560452 ) ) ;
#14525 = DIRECTION ( 'NONE',  ( 0.8660254037844379305, 0.5000000000000013323, 0.000000000000000000 ) ) ;
#14526 = DIRECTION ( 'NONE',  ( 0.000000000000000000, 0.000000000000000000, 1.000000000000000000 ) ) ;
#14527 =( LENGTH_UNIT ( ) NAMED_UNIT ( * ) SI_UNIT ( .MILLI., .METRE. ) );
#14528 = AXIS2_PLACEMENT_3D ( 'NONE', #4194, #4311, #9720 ) ;
#14529 = DIRECTION ( 'NONE',  ( -1.000000000000000000, 0.000000000000000000, 0.000000000000000000 ) ) ;
#14530 = CIRCLE ( 'NONE', #3020, 4.000000000000001776 ) ;
#14531 = CARTESIAN_POINT ( 'NONE',  ( -67.59999999999999432, 11.76776695296636888, 16.76776695296636532 ) ) ;
#14532 = DIRECTION ( 'NONE',  ( 0.000000000000000000, -0.5000000000000009992, -0.8660254037844380415 ) ) ;
#14533 = CARTESIAN_POINT ( 'NONE',  ( -3.458734124999998993, -1.432654583217642497, 17.50000000136560274 ) ) ;
#14534 = CARTESIAN_POINT ( 'NONE',  ( 4.204015924366189871, -1.626724848190933548, -3.610627190413393084 ) ) ;
#14535 = PRODUCT_DEFINITION_FORMATION_WITH_SPECIFIED_SOURCE ( 'ANY', '', #11660, .NOT_KNOWN. ) ;
#14536 = AXIS2_PLACEMENT_3D ( 'NONE', #1961, #14696, #16476 ) ;
#14537 = CARTESIAN_POINT ( 'NONE',  ( 3.458734125000001214, -1.432654583217639610, -2.574999998634404541 ) ) ;
#14538 = CARTESIAN_POINT ( 'NONE',  ( -67.40000000109247935, 10.85617417291294551, 17.06698730000000097 ) ) ;
#14539 = ADVANCED_FACE ( 'NONE', ( #20455 ), #9602, .F. ) ;
#14540 = CARTESIAN_POINT ( 'NONE',  ( -60.00000000000000711, 15.00000000000000000, 10.00000000000008882 ) ) ;
#14541 = CARTESIAN_POINT ( 'NONE',  ( 1.432654583217641164, 3.458734125000000326, 19.12500000136560629 ) ) ;
#14542 = CARTESIAN_POINT ( 'NONE',  ( 54.99999999999992895, -15.00000000000000000, 5.000000000000001776 ) ) ;
#14543 = ORIENTED_EDGE ( 'NONE', *, *, #12687, .T. ) ;
#14544 = CARTESIAN_POINT ( 'NONE',  ( -69.55000000109247082, 11.46158073645647235, 16.46158073645647235 ) ) ;
#14545 = ORIENTED_EDGE ( 'NONE', *, *, #8605, .F. ) ;
#14546 = CARTESIAN_POINT ( 'NONE',  ( 55.46643183416158962, 6.028187705514633343, 13.27509460956200016 ) ) ;
#14547 = CARTESIAN_POINT ( 'NONE',  ( -67.20000000109247651, 10.85617417291294551, 17.06698729999999742 ) ) ;
#14548 = CARTESIAN_POINT ( 'NONE',  ( -27.50000000000000711, -3.499999999999992895, -33.66025403784446723 ) ) ;
#14549 = VECTOR ( 'NONE', #3093, 1000.000000000000000 ) ;
#14550 = CARTESIAN_POINT ( 'NONE',  ( -3.458734124999999882, -1.432654583217642275, -3.199999998634404985 ) ) ;
#14551 = ORIENTED_EDGE ( 'NONE', *, *, #13145, .T. ) ;
#14552 = EDGE_CURVE ( 'NONE', #15223, #21477, #10192, .T. ) ;
#14553 = VECTOR ( 'NONE', #1505, 1000.000000000000000 ) ;
#14554 = VERTEX_POINT ( 'NONE', #21043 ) ;
#14555 = CARTESIAN_POINT ( 'NONE',  ( -60.00000000000000711, -9.999999999999998224, 25.00000000000001421 ) ) ;
#14556 = CARTESIAN_POINT ( 'NONE',  ( 53.00231816583844591, 12.07320092032949610, 12.83056023321021044 ) ) ;
#14557 = CARTESIAN_POINT ( 'NONE',  ( -69.70000000109246230, 9.143825827087049163, 17.06698729999999742 ) ) ;
#14558 = AXIS2_PLACEMENT_3D ( 'NONE', #16228, #16341, #14440 ) ;
#14559 = CARTESIAN_POINT ( 'NONE',  ( -71.55000000109245661, 8.538419263543522320, 16.46158073645647235 ) ) ;
#14560 = CARTESIAN_POINT ( 'NONE',  ( 3.458734125000001658, 1.432654583217640498, 11.25000000136560452 ) ) ;
#14561 = CARTESIAN_POINT ( 'NONE',  ( -2.828427124746188515, -2.828427124746190735, 11.25000000273119660 ) ) ;
#14562 = CARTESIAN_POINT ( 'NONE',  ( 55.31250000000000711, 13.00000000000000000, 14.99999999999998757 ) ) ;
#14563 = CYLINDRICAL_SURFACE ( 'NONE', #19390, 4.000000000000001776 ) ;
#14564 = AXIS2_PLACEMENT_3D ( 'NONE', #16687, #35, #11440 ) ;
#14565 = VECTOR ( 'NONE', #9482, 1000.000000000000000 ) ;
#14566 = CARTESIAN_POINT ( 'NONE',  ( 53.90625000000000000, 12.99999999999999645, 13.75735931288070191 ) ) ;
#14567 = LINE ( 'NONE', #5078, #4333 ) ;
#14568 = DIRECTION ( 'NONE',  ( 0.000000000000000000, 1.000000000000000000, 0.000000000000000000 ) ) ;
#14569 = CIRCLE ( 'NONE', #16077, 4.000000000000000888 ) ;
#14570 = ORIENTED_EDGE ( 'NONE', *, *, #23156, .F. ) ;
#14571 = CARTESIAN_POINT ( 'NONE',  ( -90.00000000000000000, 0.000000000000000000, -8.265000000000021885 ) ) ;
#14572 = VERTEX_POINT ( 'NONE', #8031 ) ;
#14573 = CARTESIAN_POINT ( 'NONE',  ( 52.40625000000000000, 12.99999999999999645, 13.75735931288070191 ) ) ;
#14575 = AXIS2_PLACEMENT_3D ( 'NONE', #5168, #7100, #10598 ) ;
#14574 =( NAMED_UNIT ( * ) SI_UNIT ( $, .STERADIAN. ) SOLID_ANGLE_UNIT ( ) );
#14576 = CARTESIAN_POINT ( 'NONE',  ( -2.828427124746190291, 2.828427124746190291, -3.699999997268811569 ) ) ;
#14577 = EDGE_CURVE ( 'NONE', #21889, #12232, #13996, .T. ) ;
#14578 = FACE_OUTER_BOUND ( 'NONE', #21070, .T. ) ;
#14579 = ORIENTED_EDGE ( 'NONE', *, *, #6862, .F. ) ;
#14580 = CARTESIAN_POINT ( 'NONE',  ( 2.828427124746192067, -2.828427124746189847, 17.37500000000001066 ) ) ;
#14581 = ORIENTED_EDGE ( 'NONE', *, *, #4603, .F. ) ;
#14582 = CARTESIAN_POINT ( 'NONE',  ( 45.52901028033275566, -11.25000000000000355, 10.00000000000008882 ) ) ;
#14583 = DIRECTION ( 'NONE',  ( 0.000000000000000000, 0.000000000000000000, 1.000000000000000000 ) ) ;
#14584 = ORIENTED_EDGE ( 'NONE', *, *, #11168, .T. ) ;
#14585 = DIRECTION ( 'NONE',  ( 0.000000000000000000, -1.000000000000000000, 0.000000000000000000 ) ) ;
#14586 = CYLINDRICAL_SURFACE ( 'NONE', #1791, 4.000000000000000000 ) ;
#14587 = DIRECTION ( 'NONE',  ( -1.000000000000000000, 0.000000000000000000, 0.000000000000000000 ) ) ;
#14588 = CIRCLE ( 'NONE', #6910, 8.265000000000021885 ) ;
#14589 =( GEOMETRIC_REPRESENTATION_CONTEXT ( 3 ) GLOBAL_UNCERTAINTY_ASSIGNED_CONTEXT ( ( #18878 ) ) GLOBAL_UNIT_ASSIGNED_CONTEXT ( ( #10914, #17209, #16757 ) ) REPRESENTATION_CONTEXT ( 'NONE', 'WORKASPACE' ) );
#14590 = CARTESIAN_POINT ( 'NONE',  ( 72.20000000000000284, 11.76776695296636888, 13.23223304703362579 ) ) ;
#14591 = DIRECTION ( 'NONE',  ( 1.000000000000000000, 7.703719777548943412E-32, 0.000000000000000000 ) ) ;
#14592 = FACE_OUTER_BOUND ( 'NONE', #17342, .T. ) ;
#14593 = CARTESIAN_POINT ( 'NONE',  ( 53.56481816583844591, 5.999999999999996447, 15.06805114094564502 ) ) ;
#14594 = CARTESIAN_POINT ( 'NONE',  ( 1.432654583217639832, 3.458734125000000326, -1.574999998634403875 ) ) ;
#14595 = CARTESIAN_POINT ( 'NONE',  ( -4.197393957002303999, -7.773935952363655451E-14, -3.503767560748929810 ) ) ;
#14596 = DIRECTION ( 'NONE',  ( 0.000000000000000000, -1.000000000000000000, -0.000000000000000000 ) ) ;
#14597 = VERTEX_POINT ( 'NONE', #19145 ) ;
#14598 = DIRECTION ( 'NONE',  ( -1.000000000000000000, 0.000000000000000000, 1.224646799147353454E-16 ) ) ;
#14599 = CARTESIAN_POINT ( 'NONE',  ( -3.999999999999999112, 0.000000000000000000, 11.12500000273119660 ) ) ;
#14600 = FACE_OUTER_BOUND ( 'NONE', #15545, .T. ) ;
#14601 = ORIENTED_EDGE ( 'NONE', *, *, #22231, .T. ) ;
#14602 = EDGE_LOOP ( 'NONE', ( #6164, #18400, #9716, #11685 ) ) ;
#14603 = DIRECTION ( 'NONE',  ( 0.000000000000000000, 0.000000000000000000, 1.000000000000000000 ) ) ;
#14604 = ORIENTED_EDGE ( 'NONE', *, *, #2891, .T. ) ;
#14605 = CARTESIAN_POINT ( 'NONE',  ( 55.68750000000000000, 9.999999999999978684, 10.99999999999999645 ) ) ;
#14606 = ORIENTED_EDGE ( 'NONE', *, *, #5523, .F. ) ;
#14607 = CARTESIAN_POINT ( 'NONE',  ( 118.3095189484530181, 15.00000000000003375, 34.11836509645780069 ) ) ;
#14608 = ORIENTED_EDGE ( 'NONE', *, *, #2736, .T. ) ;
#14609 = CARTESIAN_POINT ( 'NONE',  ( 55.62731816583843170, 12.87654654797634102, 17.78030770151602979 ) ) ;
#14610 = CARTESIAN_POINT ( 'NONE',  ( 68.30000000218494449, 11.76776695296636888, 13.23223304703362579 ) ) ;
#14611 = ADVANCED_FACE ( 'NONE', ( #8507 ), #13658, .F. ) ;
#14612 = DIRECTION ( 'NONE',  ( 0.000000000000000000, 0.000000000000000000, -1.000000000000000000 ) ) ;
#14613 = DIRECTION ( 'NONE',  ( -1.000000000000000000, 0.000000000000000000, 0.000000000000000000 ) ) ;
#14614 = DIRECTION ( 'NONE',  ( 0.9396926207859107594, -0.3420201433256623291, 3.697785493223492838E-32 ) ) ;
#14615 = ORIENTED_EDGE ( 'NONE', *, *, #3861, .F. ) ;
#14616 = CARTESIAN_POINT ( 'NONE',  ( -2.828427124746189403, 2.828427124746190291, 18.00000000273119483 ) ) ;
#14617 = CARTESIAN_POINT ( 'NONE',  ( -1.747541505913277282, 3.837784562140256650, -3.503702292528906526 ) ) ;
#14618 = CARTESIAN_POINT ( 'NONE',  ( 59.49768183416157541, 12.87654654797631792, 12.21969229848393113 ) ) ;
#14619 = CYLINDRICAL_SURFACE ( 'NONE', #7711, 2.500000000000002220 ) ;
#14620 = ADVANCED_FACE ( 'NONE', ( #820 ), #15463, .T. ) ;
#14621 = CARTESIAN_POINT ( 'NONE',  ( 72.50000000000000000, 9.999999999999998224, 14.99999999999999645 ) ) ;
#14622 = CARTESIAN_POINT ( 'NONE',  ( 72.15000000000001990, 11.03553390593275374, 12.50000000000001243 ) ) ;
#14623 = CARTESIAN_POINT ( 'NONE',  ( 4.000000000000000000, 4.898587196589412829E-16, -1.199999999999997957 ) ) ;
#14624 = ORIENTED_EDGE ( 'NONE', *, *, #4944, .F. ) ;
#14625 = DIRECTION ( 'NONE',  ( 1.000000000000000000, 0.000000000000000000, 0.000000000000000000 ) ) ;
#14626 = CARTESIAN_POINT ( 'NONE',  ( 55.40625000000000711, 12.99999999999999645, 13.75735931288070191 ) ) ;
#14627 = CARTESIAN_POINT ( 'NONE',  ( -3.999999999999999112, 0.000000000000000000, 17.00000000000001066 ) ) ;
#14628 = CARTESIAN_POINT ( 'NONE',  ( 0.000000000000000000, 0.000000000000000000, 0.000000000000000000 ) ) ;
#14629 = VERTEX_POINT ( 'NONE', #12104 ) ;
#14630 = DIRECTION ( 'NONE',  ( 0.000000000000000000, 0.000000000000000000, -1.000000000000000000 ) ) ;
#14631 = CARTESIAN_POINT ( 'NONE',  ( -1.432654583217640276, 3.458734125000000326, -0.4499999986344046521 ) ) ;
#14632 = CARTESIAN_POINT ( 'NONE',  ( -65.00000000000000000, 9.999999999999998224, 20.00000000000001421 ) ) ;
#14633 = VERTEX_POINT ( 'NONE', #1167 ) ;
#14634 = CARTESIAN_POINT ( 'NONE',  ( 4.999999999999999112, -9.314797388894900720, 1.239665997526853580 ) ) ;
#14635 = ORIENTED_EDGE ( 'NONE', *, *, #21550, .T. ) ;
#14636 = CYLINDRICAL_SURFACE ( 'NONE', #10279, 7.000000000000000000 ) ;
#14637 =( BOUNDED_CURVE ( )  B_SPLINE_CURVE ( 2, ( #9289, #7486, #14804, #13004, #3873, #11207, #18481, #2064, #980 ),
 .UNSPECIFIED., .F., .F. ) 
 B_SPLINE_CURVE_WITH_KNOTS ( ( 3, 2, 2, 2, 3 ),
 ( 0.000000000000000000, 0.01562499999999990459, 0.03124999999999980918, 0.04687499999999971551, 0.06249999999999961836 ),
 .UNSPECIFIED. ) 
 CURVE ( )  GEOMETRIC_REPRESENTATION_ITEM ( )  RATIONAL_B_SPLINE_CURVE ( ( 1.000000000000000000, 0.9238795325112867385, 1.000000000000000000, 0.9238795325112867385, 1.000000000000000000, 0.9238795325112867385, 1.000000000000000000, 0.9238795325112886259, 0.9999999999999981126 ) ) 
 REPRESENTATION_ITEM ( '' )  );
#14638 = CARTESIAN_POINT ( 'NONE',  ( 1.656854249492384135, -3.999999999999999112, 17.31250000000001421 ) ) ;
#14639 = DIRECTION ( 'NONE',  ( 0.5000000000000013323, -0.8660254037844379305, 0.000000000000000000 ) ) ;
#14640 = ADVANCED_FACE ( 'NONE', ( #11874 ), #697, .F. ) ;
#14641 = DIRECTION ( 'NONE',  ( 0.000000000000000000, 0.000000000000000000, -1.000000000000000000 ) ) ;
#14642 = EDGE_CURVE ( 'NONE', #23001, #4247, #57, .T. ) ;
#14643 = DIRECTION ( 'NONE',  ( 0.000000000000000000, 0.000000000000000000, -1.000000000000000000 ) ) ;
#14644 = ORIENTED_EDGE ( 'NONE', *, *, #16539, .T. ) ;
#14645 = CARTESIAN_POINT ( 'NONE',  ( -67.84999999999999432, 7.499999999999995559, 16.03553390593273420 ) ) ;
#14646 = VECTOR ( 'NONE', #2481, 1000.000000000000000 ) ;
#14647 = LINE ( 'NONE', #12847, #9175 ) ;
#14648 = ADVANCED_FACE ( 'NONE', ( #4578, #6615 ), #17515, .T. ) ;
#14649 = CARTESIAN_POINT ( 'NONE',  ( 66.75000000109247367, 8.538419263543524096, 13.53841926354352054 ) ) ;
#14650 = CARTESIAN_POINT ( 'NONE',  ( 2.445694354108821411, 2.445694354108820523, 19.06250000136560629 ) ) ;
#14651 = CARTESIAN_POINT ( 'NONE',  ( 2.000000000000001776, 0.000000000000000000, 0.000000000000000000 ) ) ;
#14652 = CARTESIAN_POINT ( 'NONE',  ( -2.828427124746189403, -2.828427124746190735, 3.425000000000002487 ) ) ;
#14653 = CARTESIAN_POINT ( 'NONE',  ( 68.55000000218494449, 11.03553390593269157, 17.50000000000004619 ) ) ;
#14654 = CARTESIAN_POINT ( 'NONE',  ( 1.872352939448454495E-15, -3.458734125000000326, 13.68750000136560629 ) ) ;
#14655 = DIRECTION ( 'NONE',  ( 0.000000000000000000, 0.000000000000000000, 1.000000000000000000 ) ) ;
#14656 = EDGE_LOOP ( 'NONE', ( #4568, #4857, #2673, #12588, #23129, #19337, #15698, #21042, #10687, #10238, #11217, #792 ) ) ;
#14657 = CARTESIAN_POINT ( 'NONE',  ( -68.60000000109248219, 12.06698729999999919, 14.14382582708705094 ) ) ;
#14658 = ORIENTED_EDGE ( 'NONE', *, *, #4864, .T. ) ;
#14659 = CARTESIAN_POINT ( 'NONE',  ( 57.90393183416158251, 14.02818770551463956, 13.41119689145323335 ) ) ;
#14660 = CARTESIAN_POINT ( 'NONE',  ( -65.65000000109247935, 9.999999999999998224, 17.06698730000000097 ) ) ;
#14661 = CARTESIAN_POINT ( 'NONE',  ( 0.000000000000000000, 0.000000000000000000, 29.99999999999998934 ) ) ;
#14662 = CARTESIAN_POINT ( 'NONE',  ( 45.00000000000000000, 10.00000000000001599, 34.11836509645782201 ) ) ;
#14663 = ORIENTED_EDGE ( 'NONE', *, *, #15357, .T. ) ;
#14664 = EDGE_CURVE ( 'NONE', #7460, #19492, #4803, .T. ) ;
#14665 = ORIENTED_EDGE ( 'NONE', *, *, #22563, .T. ) ;
#14666 = CARTESIAN_POINT ( 'NONE',  ( 0.000000000000000000, 0.000000000000000000, 0.000000000000000000 ) ) ;
#14667 = CARTESIAN_POINT ( 'NONE',  ( 51.59606816583843170, 11.17458954617364242, 11.97181229448534800 ) ) ;
#14668 = CARTESIAN_POINT ( 'NONE',  ( -71.80000000109247082, 12.06698730000000275, 14.14382582708705094 ) ) ;
#14669 = EDGE_CURVE ( 'NONE', #20897, #23413, #966, .T. ) ;
#14670 =( BOUNDED_CURVE ( )  B_SPLINE_CURVE ( 2, ( #773, #17072, #22799, #13260, #4479, #22436, #4129, #2552, #19211 ),
 .UNSPECIFIED., .F., .F. ) 
 B_SPLINE_CURVE_WITH_KNOTS ( ( 3, 2, 2, 2, 3 ),
 ( 0.1875000000000010270, 0.2031250000000009437, 0.2187500000000008327, 0.2343750000000007494, 0.2500000000000006661 ),
 .UNSPECIFIED. ) 
 CURVE ( )  GEOMETRIC_REPRESENTATION_ITEM ( )  RATIONAL_B_SPLINE_CURVE ( ( 0.9999999999999950040, 0.9238795325112917345, 1.000000000000000000, 0.9238795325112867385, 1.000000000000000000, 0.9238795325112867385, 1.000000000000000000, 0.9238795325112835188, 1.000000000000003331 ) ) 
 REPRESENTATION_ITEM ( '' )  );
#14671 = CARTESIAN_POINT ( 'NONE',  ( -71.15000000109246514, 11.46158073645647235, 13.53841926354352232 ) ) ;
#14672 = CARTESIAN_POINT ( 'NONE',  ( 2.445694354108821411, 2.445694354108820523, 11.31250000136560452 ) ) ;
#14673 = LINE ( 'NONE', #9639, #13793 ) ;
#14674 = EDGE_CURVE ( 'NONE', #5335, #21100, #19062, .T. ) ;
#14675 = CARTESIAN_POINT ( 'NONE',  ( 52.96875000000000000, 6.999999999999992895, 13.75735931288071967 ) ) ;
#14676 = CARTESIAN_POINT ( 'NONE',  ( 6.499999999999999112, 0.000000000000000000, 9.480888224575631185 ) ) ;
#14677 = ADVANCED_FACE ( 'NONE', ( #21303 ), #2997, .T. ) ;
#14678 = APPLICATION_CONTEXT ( 'automotive_design' ) ;
#14679 = CARTESIAN_POINT ( 'NONE',  ( 55.40625000000000000, 12.99999999999999645, 13.75735931288070191 ) ) ;
#14680 = CARTESIAN_POINT ( 'NONE',  ( -3.999999999999998224, -1.656854249492383246, 17.18750000273119838 ) ) ;
#14681 = DIRECTION ( 'NONE',  ( -0.000000000000000000, 1.000000000000000000, -0.000000000000000000 ) ) ;
#14682 = AXIS2_PLACEMENT_3D ( 'NONE', #23583, #1656, #3685 ) ;
#14683 = VERTEX_POINT ( 'NONE', #6842 ) ;
#14684 = CARTESIAN_POINT ( 'NONE',  ( 44.09522139676619901, -9.000000000000003553, 5.000000000000079936 ) ) ;
#14685 = LINE ( 'NONE', #11086, #18151 ) ;
#14686 = ORIENTED_EDGE ( 'NONE', *, *, #6636, .F. ) ;
#14687 = CARTESIAN_POINT ( 'NONE',  ( 54.37500000000000711, 7.878679656440349177, 12.87867965644035984 ) ) ;
#14688 = CARTESIAN_POINT ( 'NONE',  ( -4.000000000000000000, 0.000000000000000000, -2.574999997268812457 ) ) ;
#14689 = AXIS2_PLACEMENT_3D ( 'NONE', #623, #11918, #19186 ) ;
#14690 = FACE_OUTER_BOUND ( 'NONE', #1193, .T. ) ;
#14691 = ORIENTED_EDGE ( 'NONE', *, *, #16566, .T. ) ;
#14692 = CARTESIAN_POINT ( 'NONE',  ( 4.000000000000000888, 1.656854249492381248, 15.56250000000000888 ) ) ;
#14693 = CARTESIAN_POINT ( 'NONE',  ( 2.828427124746190735, -2.828427124746189847, -2.324999999999998845 ) ) ;
#14694 = CARTESIAN_POINT ( 'NONE',  ( 68.99999999999998579, 11.76776695296636888, 13.23223304703362579 ) ) ;
#14695 = VERTEX_POINT ( 'NONE', #19287 ) ;
#14696 = DIRECTION ( 'NONE',  ( 1.224646799147353207E-16, -0.000000000000000000, 1.000000000000000000 ) ) ;
#14697 = CLOSED_SHELL ( 'NONE', ( #17278, #20477, #283, #6938, #9645, #21223, #19584, #16645, #20462, #9893, #687, #17871, #23000, #5567, #7901, #8655, #2769, #3237, #17857, #17736, #8360, #8650, #8324, #4500, #17313, #12193, #4234, #12460, #12023, #6839, #22287, #9328, #23381, #3999, #12525, #9765, #18032, #10034, #14131, #3951, #13172, #3235, #2035, #15267, #3359, #8841 ) ) ;
#14698 = LINE ( 'NONE', #3761, #7563 ) ;
#14699 = CARTESIAN_POINT ( 'NONE',  ( -2.445694354108820523, 2.445694354108820523, 1.862500001365596347 ) ) ;
#14700 = CIRCLE ( 'NONE', #22704, 5.000000000000011546 ) ;
#14701 = CARTESIAN_POINT ( 'NONE',  ( 67.74999999999998579, 8.964466094067258695, 17.50000000000000355 ) ) ;
#14702 = EDGE_CURVE ( 'NONE', #6515, #17055, #8362, .T. ) ;
#14703 = FACE_OUTER_BOUND ( 'NONE', #18105, .T. ) ;
#14704 = ADVANCED_FACE ( 'NONE', ( #15497 ), #11171, .T. ) ;
#14705 = DIRECTION ( 'NONE',  ( -1.000000000000000000, 0.000000000000000000, -0.000000000000000000 ) ) ;
#14706 = CARTESIAN_POINT ( 'NONE',  ( 52.15856816583843880, 6.028187705514649330, 16.72490539043803182 ) ) ;
#14707 = CARTESIAN_POINT ( 'NONE',  ( -3.458734125000000326, 0.000000000000000000, 0.7375000013655954589 ) ) ;
#14708 = CARTESIAN_POINT ( 'NONE',  ( 3.458734125000001658, 1.432654583217640498, 19.25000000136560274 ) ) ;
#14709 = DIRECTION ( 'NONE',  ( 0.000000000000000000, 0.000000000000000000, 1.000000000000000000 ) ) ;
#14710 = CARTESIAN_POINT ( 'NONE',  ( -1.656854249492380582, 4.000000000000000000, 0.1125000000000017791 ) ) ;
#14711 = CARTESIAN_POINT ( 'NONE',  ( -3.999999999999999112, 0.000000000000000000, 17.00000000000001066 ) ) ;
#14712 = ORIENTED_EDGE ( 'NONE', *, *, #11617, .F. ) ;
#14713 = FACE_BOUND ( 'NONE', #3524, .T. ) ;
#14714 = CARTESIAN_POINT ( 'NONE',  ( -10.00000000000000000, 0.000000000000000000, 0.000000000000000000 ) ) ;
#14715 = CARTESIAN_POINT ( 'NONE',  ( -4.736472119667250347, -11.25000000000000355, 5.000000000000079936 ) ) ;
#14716 = VERTEX_POINT ( 'NONE', #7445 ) ;
#14717 = VERTEX_POINT ( 'NONE', #9135 ) ;
#14718 = ORIENTED_EDGE ( 'NONE', *, *, #1145, .T. ) ;
#14719 = CARTESIAN_POINT ( 'NONE',  ( 53.34375000000000000, 8.343145750507636293, 19.00000000000000000 ) ) ;
#14720 = ORIENTED_EDGE ( 'NONE', *, *, #21094, .F. ) ;
#14721 = DIRECTION ( 'NONE',  ( 0.000000000000000000, 0.000000000000000000, -1.000000000000000000 ) ) ;
#14722 = ORIENTED_EDGE ( 'NONE', *, *, #1603, .F. ) ;
#14723 = CARTESIAN_POINT ( 'NONE',  ( 53.09606816583843170, 11.58880310854672935, 10.97181229448534445 ) ) ;
#14724 = CARTESIAN_POINT ( 'NONE',  ( 65.80000000218494449, 9.999999999999998224, 12.49999999999999289 ) ) ;
#14725 = MANIFOLD_SOLID_BREP ( 'Keyway', #1262 ) ;
#14726 = AXIS2_PLACEMENT_3D ( 'NONE', #15335, #1034, #15449 ) ;
#14727 = DIRECTION ( 'NONE',  ( 0.000000000000000000, 0.000000000000000000, -1.000000000000000000 ) ) ;
#14728 = DIRECTION ( 'NONE',  ( 0.3420201433256622736, 0.9396926207859106484, 0.000000000000000000 ) ) ;
#14729 = CARTESIAN_POINT ( 'NONE',  ( -5.384454397937118664, 6.594054843588581554E-16, -4.484454397937119197 ) ) ;
#14730 = VERTEX_POINT ( 'NONE', #19988 ) ;
#14731 = CARTESIAN_POINT ( 'NONE',  ( 1.656854249492381470, 4.000000000000000000, 16.81250000273119838 ) ) ;
#14732 = CARTESIAN_POINT ( 'NONE',  ( 45.00000000000000000, -15.00000000000003375, 34.11836509645780779 ) ) ;
#14733 = CARTESIAN_POINT ( 'NONE',  ( 59.25000000000000711, 7.171572875253819923, 17.82842712474619873 ) ) ;
#14734 = CARTESIAN_POINT ( 'NONE',  ( 2.697128823393878605, -5.948365447239590154, -3.686277791023379713 ) ) ;
#14735 = CARTESIAN_POINT ( 'NONE',  ( 66.90000000218495302, 11.76776695296636888, 16.76776695296636532 ) ) ;
#14736 = CARTESIAN_POINT ( 'NONE',  ( -3.250000000000003997, -5.629165124598848102, 1.734723475976807094E-15 ) ) ;
#14737 = DIRECTION ( 'NONE',  ( -0.000000000000000000, -0.000000000000000000, 1.000000000000000000 ) ) ;
#14738 = ORIENTED_EDGE ( 'NONE', *, *, #1017, .F. ) ;
#14739 = FACE_OUTER_BOUND ( 'NONE', #23385, .T. ) ;
#14740 = CARTESIAN_POINT ( 'NONE',  ( -4.000000000000000000, 2.471528634177585282, -3.686887442155186712 ) ) ;
#14741 = DIRECTION ( 'NONE',  ( 0.000000000000000000, 0.000000000000000000, 1.000000000000000000 ) ) ;
#14742 =( LENGTH_UNIT ( ) NAMED_UNIT ( * ) SI_UNIT ( .MILLI., .METRE. ) );
#14743 = AXIS2_PLACEMENT_3D ( 'NONE', #17735, #17630, #19517 ) ;
#14744 = VERTEX_POINT ( 'NONE', #18091 ) ;
#14745 = EDGE_CURVE ( 'NONE', #20280, #20897, #14759, .T. ) ;
#14746 = CYLINDRICAL_SURFACE ( 'NONE', #20842, 8.073750000000021743 ) ;
#14747 = CARTESIAN_POINT ( 'NONE',  ( 2.500000000000000000, 2.357898499370431722, -2.818925648462311528E-15 ) ) ;
#14748 = CARTESIAN_POINT ( 'NONE',  ( 1.144235203016666258, 3.958177651039090250, -0.09382832055445661235 ) ) ;
#14749 = CIRCLE ( 'NONE', #9370, 4.999999999999999112 ) ;
#14750 = ORIENTED_EDGE ( 'NONE', *, *, #2501, .T. ) ;
#14751 = CARTESIAN_POINT ( 'NONE',  ( -65.00000000000000000, 15.00000000000000000, 10.00000000000008882 ) ) ;
#14752 = ORIENTED_EDGE ( 'NONE', *, *, #3363, .F. ) ;
#14753 = ORIENTED_EDGE ( 'NONE', *, *, #6906, .T. ) ;
#14754 = CARTESIAN_POINT ( 'NONE',  ( 21.28513981966725765, -11.25000000000000355, 5.000000000000079936 ) ) ;
#14755 = CARTESIAN_POINT ( 'NONE',  ( -3.458734124999998993, -1.432654583217642497, 10.75000000136560452 ) ) ;
#14756 = CARTESIAN_POINT ( 'NONE',  ( 2.435583919667260400, -11.25000000000000355, 5.000000000000079936 ) ) ;
#14757 = CARTESIAN_POINT ( 'NONE',  ( 0.000000000000000000, 0.000000000000000000, -3.700000000000000178 ) ) ;
#14758 = DIRECTION ( 'NONE',  ( 1.000000000000000000, 0.000000000000000000, 0.000000000000000000 ) ) ;
#14759 = LINE ( 'NONE', #3591, #17162 ) ;
#14760 = ORIENTED_EDGE ( 'NONE', *, *, #1937, .T. ) ;
#14761 = AXIS2_PLACEMENT_3D ( 'NONE', #16061, #6715, #2866 ) ;
#14762 = CARTESIAN_POINT ( 'NONE',  ( -60.00000000000000711, 9.999999999999998224, 17.49999999999999645 ) ) ;
#14763 = AXIS2_PLACEMENT_3D ( 'NONE', #22237, #20438, #4047 ) ;
#14764 = CARTESIAN_POINT ( 'NONE',  ( 2.828427124746190735, -2.828427124746189847, -0.1999999972688119854 ) ) ;
#14765 = CARTESIAN_POINT ( 'NONE',  ( 66.90000000109246514, 10.85617417291294551, 12.93301269999999370 ) ) ;
#14766 = MANIFOLD_SOLID_BREP ( 'InnerRace', #899 ) ;
#14767 = CARTESIAN_POINT ( 'NONE',  ( -1.432654583217638944, 3.458734125000000326, 19.25000000136560274 ) ) ;
#14768 = CARTESIAN_POINT ( 'NONE',  ( 33.85151041966726382, -11.25000000000000355, 5.000000000000079936 ) ) ;
#14769 = CARTESIAN_POINT ( 'NONE',  ( -2.828427124746190291, 2.828427124746190291, 5.175000000000000711 ) ) ;
#14770 = CARTESIAN_POINT ( 'NONE',  ( 4.000000000000000888, 4.898587196589412829E-16, 12.50000000000001066 ) ) ;
#14771 = CARTESIAN_POINT ( 'NONE',  ( 3.458734125000001214, 1.432654583217640498, 12.00000000136560452 ) ) ;
#14772 = LINE ( 'NONE', #12975, #19509 ) ;
#14773 = ORIENTED_EDGE ( 'NONE', *, *, #8220, .F. ) ;
#14774 = ADVANCED_FACE ( 'NONE', ( #19758 ), #4911, .T. ) ;
#14775 = CARTESIAN_POINT ( 'NONE',  ( -67.55000000109247082, 8.538419263543524096, 13.53841926354352054 ) ) ;
#14776 = EDGE_LOOP ( 'NONE', ( #762, #10886, #22494, #20781 ) ) ;
#14777 = CARTESIAN_POINT ( 'NONE',  ( 57.24768183416158962, 7.123453452023678523, 17.78030770151605822 ) ) ;
#14778 = CARTESIAN_POINT ( 'NONE',  ( -70.75000000109247367, 8.538419263543522320, 16.46158073645647235 ) ) ;
#14779 = APPLICATION_PROTOCOL_DEFINITION ( 'draft international standard', 'automotive_design', 1998, #12856 ) ;
#14780 =( BOUNDED_CURVE ( )  B_SPLINE_CURVE ( 2, ( #319, #13052, #2233, #7879, #5836, #15087, #22342, #11136, #14974 ),
 .UNSPECIFIED., .F., .F. ) 
 B_SPLINE_CURVE_WITH_KNOTS ( ( 3, 2, 2, 2, 3 ),
 ( 0.9375000000000007772, 0.9531250000000005551, 0.9687500000000004441, 0.9843750000000002220, 1.000000000000000000 ),
 .UNSPECIFIED. ) 
 CURVE ( )  GEOMETRIC_REPRESENTATION_ITEM ( )  RATIONAL_B_SPLINE_CURVE ( ( 0.9999999999999962252, 0.9238795325112905132, 1.000000000000000000, 0.9238795325112867385, 1.000000000000000000, 0.9238795325112867385, 1.000000000000000000, 0.9238795325112867385, 1.000000000000000000 ) ) 
 REPRESENTATION_ITEM ( '' )  );
#14781 = EDGE_CURVE ( 'NONE', #1631, #12232, #3483, .T. ) ;
#14782 = CARTESIAN_POINT ( 'NONE',  ( 4.000000000000000000, 4.898587196589412829E-16, 0.9250000027311873207 ) ) ;
#14783 = ORIENTED_EDGE ( 'NONE', *, *, #3205, .F. ) ;
#14784 = AXIS2_PLACEMENT_3D ( 'NONE', #5530, #3609, #1930 ) ;
#14785 = VECTOR ( 'NONE', #20939, 1000.000000000000000 ) ;
#14786 = ORIENTED_EDGE ( 'NONE', *, *, #4661, .T. ) ;
#14787 = AXIS2_PLACEMENT_3D ( 'NONE', #13767, #23069, #13526 ) ;
#14788 = CARTESIAN_POINT ( 'NONE',  ( 3.458734125000002546, -1.432654583217639610, 19.12500000136560629 ) ) ;
#14789 = ADVANCED_FACE ( 'NONE', ( #12618 ), #3702, .F. ) ;
#14790 = CARTESIAN_POINT ( 'NONE',  ( 53.18981816583844591, 9.931948859054354983, 11.99999999999999645 ) ) ;
#14791 = CARTESIAN_POINT ( 'NONE',  ( -71.45000000109247651, 7.933012699999995476, 14.99999999999999645 ) ) ;
#14792 = CARTESIAN_POINT ( 'NONE',  ( -70.55000000109245661, 11.46158073645647235, 16.46158073645647235 ) ) ;
#14793 = DIRECTION ( 'NONE',  ( 0.000000000000000000, 0.000000000000000000, -1.000000000000000000 ) ) ;
#14794 = CARTESIAN_POINT ( 'NONE',  ( 29.00211400323381028, -9.000000000000005329, 10.00000000000008882 ) ) ;
#14795 = CARTESIAN_POINT ( 'NONE',  ( 51.46875000000000000, 6.999999999999992895, 13.75735931288071967 ) ) ;
#14796 = CARTESIAN_POINT ( 'NONE',  ( -65.00000000000000000, 15.00000000000000000, 25.00000000000001421 ) ) ;
#14797 = CARTESIAN_POINT ( 'NONE',  ( 51.75000000000000711, 7.878679656440361612, 17.12132034355964549 ) ) ;
#14798 = EDGE_CURVE ( 'NONE', #14897, #10661, #21333, .T. ) ;
#14799 = CARTESIAN_POINT ( 'NONE',  ( 4.000000000000000888, 1.656854249492381248, 15.68750000273119660 ) ) ;
#14800 = CARTESIAN_POINT ( 'NONE',  ( 1.567478505476134606E-15, 4.618802153517012066, -3.433295621305382905 ) ) ;
#14801 = VERTEX_POINT ( 'NONE', #21901 ) ;
#14802 = DIRECTION ( 'NONE',  ( 1.000000000000000000, 0.000000000000000000, 0.000000000000000000 ) ) ;
#14803 = EDGE_CURVE ( 'NONE', #2788, #9234, #2497, .T. ) ;
#14804 = CARTESIAN_POINT ( 'NONE',  ( -71.70000000218495018, 11.76776695296636888, 16.76776695296636532 ) ) ;
#14805 = ORIENTED_EDGE ( 'NONE', *, *, #21184, .T. ) ;
#14806 = CARTESIAN_POINT ( 'NONE',  ( 56.34375000000000711, 8.757359312880723223, 18.00000000000000355 ) ) ;
#14807 = CARTESIAN_POINT ( 'NONE',  ( -2.117863837641485618E-16, 3.458734125000000326, 5.487500001365596347 ) ) ;
#14808 = EDGE_CURVE ( 'NONE', #5642, #16821, #14109, .T. ) ;
#14809 = CARTESIAN_POINT ( 'NONE',  ( 0.2615509004163102946, 3.991439731035835603, 2.039999999999998259 ) ) ;
#14810 = VERTEX_POINT ( 'NONE', #21517 ) ;
#14811 = CARTESIAN_POINT ( 'NONE',  ( -1.656854249492379250, 4.000000000000000000, 15.81250000000001066 ) ) ;
#14812 = CARTESIAN_POINT ( 'NONE',  ( 18.14354716966726144, -11.25000000000000355, 5.000000000000079936 ) ) ;
#14813 = CARTESIAN_POINT ( 'NONE',  ( 69.29999999999999716, 9.999999999999998224, 17.49999999999999645 ) ) ;
#14814 = ORIENTED_EDGE ( 'NONE', *, *, #13048, .T. ) ;
#14815 = EDGE_CURVE ( 'NONE', #5234, #16245, #2609, .T. ) ;
#14816 = EDGE_CURVE ( 'NONE', #18435, #12712, #16507, .T. ) ;
#14817 = DIRECTION ( 'NONE',  ( -0.000000000000000000, 1.000000000000000000, -0.000000000000000000 ) ) ;
#14818 = CARTESIAN_POINT ( 'NONE',  ( -1.432654583217640498, 3.458734125000000770, -0.1999999986344043745 ) ) ;
#14819 = CARTESIAN_POINT ( 'NONE',  ( 67.45000000000000284, 12.50000000000000000, 13.96446609406725869 ) ) ;
#14820 = CARTESIAN_POINT ( 'NONE',  ( -2.697128823393878161, 5.948365447239581272, -3.686277791023383710 ) ) ;
#14821 = DIRECTION ( 'NONE',  ( 0.000000000000000000, -6.982962677686266711E-15, 1.000000000000000000 ) ) ;
#14822 = CARTESIAN_POINT ( 'NONE',  ( 51.50231816583844591, 12.78030770151603868, 12.12345345202365188 ) ) ;
#14823 = CARTESIAN_POINT ( 'NONE',  ( -2.445694354108819635, -2.445694354108820523, 0.8625000013655955700 ) ) ;
#14824 = CARTESIAN_POINT ( 'NONE',  ( 1.025207404391860050E-15, 3.458734125000000770, 14.43750000136560452 ) ) ;
#14825 = CARTESIAN_POINT ( 'NONE',  ( -71.79999999999998295, 8.232233047033627571, 16.76776695296636532 ) ) ;
#14826 = DIRECTION ( 'NONE',  ( 1.000000000000000000, 0.000000000000000000, 0.000000000000000000 ) ) ;
#14827 = CARTESIAN_POINT ( 'NONE',  ( -1.656854249492379472, 4.000000000000000000, 16.81250000000001066 ) ) ;
#14828 = VERTEX_POINT ( 'NONE', #7180 ) ;
#14829 = CARTESIAN_POINT ( 'NONE',  ( 0.000000000000000000, -1.699438267350438903, 9.241976615262153416 ) ) ;
#14830 = CARTESIAN_POINT ( 'NONE',  ( 1.655952806101427033, -3.662737355149048302, -1.182683869819604841E-14 ) ) ;
#14831 = ADVANCED_FACE ( 'NONE', ( #20075 ), #16164, .F. ) ;
#14832 = DIRECTION ( 'NONE',  ( -1.000000000000000000, 0.000000000000000000, 0.000000000000000000 ) ) ;
#14833 = ORIENTED_EDGE ( 'NONE', *, *, #316, .T. ) ;
#14834 = EDGE_LOOP ( 'NONE', ( #1548, #16696, #22835, #15557 ) ) ;
#14835 = SURFACE_SIDE_STYLE ('',( #434 ) ) ;
#14836 = ADVANCED_FACE ( 'NONE', ( #1646 ), #5243, .F. ) ;
#14837 = CARTESIAN_POINT ( 'NONE',  ( 56.62500000000000000, 12.82842712474620228, 17.82842712474617386 ) ) ;
#14838 = VERTEX_POINT ( 'NONE', #14495 ) ;
#14839 = CARTESIAN_POINT ( 'NONE',  ( -3.999999999999998224, -1.656854249492383024, 18.06250000000001421 ) ) ;
#14840 = ORIENTED_EDGE ( 'NONE', *, *, #9071, .F. ) ;
#14841 = AXIS2_PLACEMENT_3D ( 'NONE', #10782, #15912, #5115 ) ;
#14842 = ADVANCED_FACE ( 'NONE', ( #19849 ), #3209, .T. ) ;
#14843 = CARTESIAN_POINT ( 'NONE',  ( 57.22106816583844591, 14.02818770551465377, 16.58880310854672757 ) ) ;
#14844 = CARTESIAN_POINT ( 'NONE',  ( 70.40000000109250777, 10.85617417291294551, 17.06698729999999742 ) ) ;
#14845 = VECTOR ( 'NONE', #12653, 1000.000000000000000 ) ;
#14846 = PLANE ( 'NONE',  #5355 ) ;
#14847 = CARTESIAN_POINT ( 'NONE',  ( 70.65000000109246514, 9.999999999999998224, 17.06698730000000097 ) ) ;
#14848 = EDGE_LOOP ( 'NONE', ( #13866, #7864, #12800, #18031 ) ) ;
#14849 = CARTESIAN_POINT ( 'NONE',  ( 1.656854249492381470, 4.000000000000000000, 17.81250000273119483 ) ) ;
#14850 = VECTOR ( 'NONE', #23200, 1000.000000000000000 ) ;
#14851 = DIRECTION ( 'NONE',  ( 0.000000000000000000, 0.000000000000000000, -1.000000000000000000 ) ) ;
#14852 = CARTESIAN_POINT ( 'NONE',  ( 54.90393183416157541, 14.02818770551463956, 13.41119689145323335 ) ) ;
#14853 = CARTESIAN_POINT ( 'NONE',  ( 3.349393607134518280, 2.131150051602727302, 2.039999999999998259 ) ) ;
#14854 = DIRECTION ( 'NONE',  ( -7.087422195345011518E-32, -1.000000000000000000, -0.000000000000000000 ) ) ;
#14855 = AXIS2_PLACEMENT_3D ( 'NONE', #23440, #9088, #10660 ) ;
#14856 = CARTESIAN_POINT ( 'NONE',  ( 72.39999999999999147, 11.76776695296636888, 16.76776695296636532 ) ) ;
#14857 = AXIS2_PLACEMENT_3D ( 'NONE', #5061, #6986, #7790 ) ;
#14858 = CARTESIAN_POINT ( 'NONE',  ( 4.203935335434060505, 1.640780671294165272, -3.598452447879202598 ) ) ;
#14859 = EDGE_LOOP ( 'NONE', ( #14378, #21126 ) ) ;
#14860 = DIRECTION ( 'NONE',  ( -1.000000000000000000, 0.000000000000000000, -0.000000000000000000 ) ) ;
#14861 = CARTESIAN_POINT ( 'NONE',  ( -4.211405944401398038, -2.460460786169389902, -3.751298493805494072 ) ) ;
#14862 = DIRECTION ( 'NONE',  ( 1.000000000000000000, 0.000000000000000000, 0.000000000000000000 ) ) ;
#14863 = DIRECTION ( 'NONE',  ( 0.000000000000000000, 0.000000000000000000, 1.000000000000000000 ) ) ;
#14864 = ORIENTED_EDGE ( 'NONE', *, *, #19748, .T. ) ;
#14865 = CARTESIAN_POINT ( 'NONE',  ( -4.000000000000000000, -7.806255641895631925E-15, -3.142992957459232350 ) ) ;
#14866 = CARTESIAN_POINT ( 'NONE',  ( 70.50000000000000000, 9.999999999999998224, 12.49999999999999289 ) ) ;
#14867 = CARTESIAN_POINT ( 'NONE',  ( -6.500000000000000000, 3.145973671264222116, -0.4053876232513699551 ) ) ;
#14868 = EDGE_CURVE ( 'NONE', #7079, #7525, #9873, .T. ) ;
#14869 = CARTESIAN_POINT ( 'NONE',  ( 0.000000000000000000, 0.000000000000000000, 0.000000000000000000 ) ) ;
#14870 = ORIENTED_EDGE ( 'NONE', *, *, #4248, .F. ) ;
#14871 = DIRECTION ( 'NONE',  ( -1.000000000000000000, 0.000000000000000000, 1.224646799147353207E-16 ) ) ;
#14872 = VERTEX_POINT ( 'NONE', #11012 ) ;
#14873 = CIRCLE ( 'NONE', #13700, 4.000000000000000000 ) ;
#14874 = DIRECTION ( 'NONE',  ( 0.3420201433256622181, 0.9396926207859107594, -6.162975822039141593E-32 ) ) ;
#14875 = CARTESIAN_POINT ( 'NONE',  ( -2.828427124746188515, -2.828427124746190735, 16.12500000000001066 ) ) ;
#14876 = DIRECTION ( 'NONE',  ( -1.000000000000000000, 0.000000000000000000, -0.000000000000000000 ) ) ;
#14877 = CIRCLE ( 'NONE', #12195, 4.000000000000001776 ) ;
#14878 = AXIS2_PLACEMENT_3D ( 'NONE', #10016, #2785, #11810 ) ;
#14879 = CYLINDRICAL_SURFACE ( 'NONE', #19855, 5.000000000000011546 ) ;
#14880 = MECHANICAL_DESIGN_GEOMETRIC_PRESENTATION_REPRESENTATION (  '', ( #10302 ), #13726 ) ;
#14881 = CARTESIAN_POINT ( 'NONE',  ( 4.000000000000000888, 4.898587196589412829E-16, 17.62500000273119483 ) ) ;
#14882 = CARTESIAN_POINT ( 'NONE',  ( 70.10000000109246798, 7.933012699999995476, 14.14382582708705094 ) ) ;
#14883 = ORIENTED_EDGE ( 'NONE', *, *, #10439, .T. ) ;
#14884 = LINE ( 'NONE', #11173, #714 ) ;
#14885 = FACE_OUTER_BOUND ( 'NONE', #16642, .T. ) ;
#14886 = CARTESIAN_POINT ( 'NONE',  ( 68.05000000109247082, 9.999999999999998224, 17.06698730000000097 ) ) ;
#14887 = CARTESIAN_POINT ( 'NONE',  ( 2.445694354108821411, 2.445694354108820523, 16.06250000136560629 ) ) ;
#14888 = DIRECTION ( 'NONE',  ( -1.224646799147353207E-16, 0.000000000000000000, -1.000000000000000000 ) ) ;
#14889 = DIRECTION ( 'NONE',  ( -1.000000000000000000, 0.000000000000000000, 0.000000000000000000 ) ) ;
#14890 = CARTESIAN_POINT ( 'NONE',  ( 1.656854249492380360, 4.000000000000000000, 4.987500000000000711 ) ) ;
#14891 = CARTESIAN_POINT ( 'NONE',  ( 4.999999999999999112, 0.000000000000000000, 0.000000000000000000 ) ) ;
#14892 = CARTESIAN_POINT ( 'NONE',  ( 3.458734125000001214, 4.235727675282971730E-16, 12.93750000136560452 ) ) ;
#14893 = CARTESIAN_POINT ( 'NONE',  ( -67.05000000218494449, 8.964466094067246260, 17.49999999999999289 ) ) ;
#14894 = PRODUCT_DEFINITION_SHAPE ( 'NONE', 'NONE',  #13574 ) ;
#14895 = VERTEX_POINT ( 'NONE', #21875 ) ;
#14896 = CARTESIAN_POINT ( 'NONE',  ( -70.00000000109247367, 9.143825827087052716, 12.93301269999999192 ) ) ;
#14897 = VERTEX_POINT ( 'NONE', #8737 ) ;
#14898 = CARTESIAN_POINT ( 'NONE',  ( 58.78125000000000711, 8.343145750507600766, 11.00000000000000533 ) ) ;
#14899 = CARTESIAN_POINT ( 'NONE',  ( -71.45000000109247651, 9.999999999999998224, 17.06698730000000097 ) ) ;
#14900 = APPLICATION_PROTOCOL_DEFINITION ( 'draft international standard', 'automotive_design', 1998, #1177 ) ;
#14901 = VECTOR ( 'NONE', #21979, 1000.000000000000114 ) ;
#14902 = DIRECTION ( 'NONE',  ( 0.3420201433256622181, -0.9396926207859107594, 0.000000000000000000 ) ) ;
#14903 = ORIENTED_EDGE ( 'NONE', *, *, #7309, .F. ) ;
#14904 = VERTEX_POINT ( 'NONE', #18066 ) ;
#14905 = CARTESIAN_POINT ( 'NONE',  ( 1.432654583217643163, -3.458734124999999882, 16.00000000136560629 ) ) ;
#14906 = CARTESIAN_POINT ( 'NONE',  ( 53.34375000000000000, 8.757359312880723223, 18.00000000000000355 ) ) ;
#14907 = AXIS2_PLACEMENT_3D ( 'NONE', #10900, #6943, #10671 ) ;
#14908 = CARTESIAN_POINT ( 'NONE',  ( -69.85000000109248219, 7.933012699999995476, 14.99999999999999645 ) ) ;
#14909 = PRODUCT_DEFINITION_FORMATION_WITH_SPECIFIED_SOURCE ( 'ANY', '', #2634, .NOT_KNOWN. ) ;
#14910 = EDGE_CURVE ( 'NONE', #13512, #13219, #1762, .T. ) ;
#14911 = CARTESIAN_POINT ( 'NONE',  ( -69.05000000109247082, 9.999999999999998224, 17.06698730000000097 ) ) ;
#14912 = VECTOR ( 'NONE', #21721, 1000.000000000000000 ) ;
#14913 = CARTESIAN_POINT ( 'NONE',  ( -1.432654583217639166, 3.458734125000000770, 11.50000000136560452 ) ) ;
#14914 = CARTESIAN_POINT ( 'NONE',  ( -18.72738675928344065, -8.974600000000002353, 5.000000000000079936 ) ) ;
#14915 = CARTESIAN_POINT ( 'NONE',  ( 60.62268183416157541, 12.07320092032950676, 17.16943976678977180 ) ) ;
#14916 = CARTESIAN_POINT ( 'NONE',  ( 72.04999999999998295, 8.964466094067278235, 12.49999999999997691 ) ) ;
#14917 = EDGE_CURVE ( 'NONE', #16269, #4081, #4926, .T. ) ;
#14918 =( BOUNDED_CURVE ( )  B_SPLINE_CURVE ( 2, ( #2953, #10307, #15804, #5358, #8607, #8980, #1518, #23676, #1270 ),
 .UNSPECIFIED., .F., .F. ) 
 B_SPLINE_CURVE_WITH_KNOTS ( ( 3, 2, 2, 2, 3 ),
 ( 0.5000000000000000000, 0.5124999999999999556, 0.5250000000000000222, 0.5374999999999999778, 0.5500000000000000444 ),
 .UNSPECIFIED. ) 
 CURVE ( )  GEOMETRIC_REPRESENTATION_ITEM ( )  RATIONAL_B_SPLINE_CURVE ( ( 1.000000000000000000, 0.9238795325112867385, 1.000000000000000000, 0.9238795325112867385, 1.000000000000000000, 0.9238795325112867385, 1.000000000000000000, 0.9238795325112867385, 1.000000000000000000 ) ) 
 REPRESENTATION_ITEM ( '' )  );
#14919 = CARTESIAN_POINT ( 'NONE',  ( 53.34375000000000000, 8.757359312880723223, 18.00000000000000355 ) ) ;
#14920 = CARTESIAN_POINT ( 'NONE',  ( -3.458734124999998993, 0.000000000000000000, 11.43750000136560452 ) ) ;
#14921 = B_SPLINE_CURVE_WITH_KNOTS ( 'NONE', 3,
 ( #9819, #7898, #11865, #15103, #22723, #20803 ),
 .UNSPECIFIED., .F., .F.,
 ( 4, 2, 4 ),
 ( 0.000000000000000000, 0.0002095117440854730670, 0.0004190234881709461339 ),
 .UNSPECIFIED. ) ;
#14922 = CARTESIAN_POINT ( 'NONE',  ( -1.656854249492380138, -3.999999999999999112, 15.31250000273119660 ) ) ;
#14923 = AXIS2_PLACEMENT_3D ( 'NONE', #9133, #5, #12499 ) ;
#14924 = EDGE_CURVE ( 'NONE', #11955, #19365, #12989, .T. ) ;
#14925 = CARTESIAN_POINT ( 'NONE',  ( -69.35000000218497007, 11.03553390593273420, 17.50000000000000711 ) ) ;
#14926 = AXIS2_PLACEMENT_3D ( 'NONE', #10557, #1399, #2851 ) ;
#14927 = ORIENTED_EDGE ( 'NONE', *, *, #6597, .T. ) ;
#14928 = DIRECTION ( 'NONE',  ( 0.000000000000000000, 0.000000000000000000, -1.000000000000000000 ) ) ;
#14929 = CARTESIAN_POINT ( 'NONE',  ( 0.1756481739660539498, -4.720212674038995360, -3.469390959564070620 ) ) ;
#14930 = EDGE_LOOP ( 'NONE', ( #18961, #2946, #11504, #23281 ) ) ;
#14931 = CARTESIAN_POINT ( 'NONE',  ( 56.71875000000000711, 13.00000000000000711, 16.24264068711927322 ) ) ;
#14932 = CARTESIAN_POINT ( 'NONE',  ( 1.432654583217642275, -3.458734124999999437, 4.050000001365596347 ) ) ;
#14933 = DIRECTION ( 'NONE',  ( 0.000000000000000000, -5.754033390038003495E-16, 1.000000000000000000 ) ) ;
#14934 = EDGE_LOOP ( 'NONE', ( #22488, #9881, #23621, #14021 ) ) ;
#14935 = CARTESIAN_POINT ( 'NONE',  ( -3.999999999999999112, 0.000000000000000000, 13.00000000000001066 ) ) ;
#14936 = DIRECTION ( 'NONE',  ( -1.000000000000000000, -0.000000000000000000, -0.000000000000000000 ) ) ;
#14937 = CIRCLE ( 'NONE', #385, 4.999999999999999112 ) ;
#14938 = CARTESIAN_POINT ( 'NONE',  ( -19.99999999999999645, -9.000000000000003553, 5.000000000000079936 ) ) ;
#14939 = EDGE_LOOP ( 'NONE', ( #6944, #2840, #23653, #7739, #12186, #21717, #19744, #9378, #22633, #7903, #13549, #1327 ) ) ;
#14940 = CARTESIAN_POINT ( 'NONE',  ( 4.999999999999999112, 1.699438267350500409, -9.241976615262139205 ) ) ;
#14941 = CARTESIAN_POINT ( 'NONE',  ( 6.353591512924457348E-16, -3.458734125000000770, 1.237500001365595903 ) ) ;
#14942 = AXIS2_PLACEMENT_3D ( 'NONE', #5574, #14349, #7278 ) ;
#14943 = EDGE_CURVE ( 'NONE', #9577, #17502, #13367, .T. ) ;
#14944 = CARTESIAN_POINT ( 'NONE',  ( 68.29999999999999716, 12.50000000000000000, 14.99999999999999645 ) ) ;
#14945 = EDGE_CURVE ( 'NONE', #16266, #2194, #19449, .T. ) ;
#14946 = CARTESIAN_POINT ( 'NONE',  ( -2.149058192116894084, 6.264794173742276762, -3.633174458636620141 ) ) ;
#14947 = CIRCLE ( 'NONE', #8461, 2.041999999999999815 ) ;
#14948 = DIRECTION ( 'NONE',  ( 1.000000000000000000, 7.703719777548943412E-32, 0.000000000000000000 ) ) ;
#14949 = AXIS2_PLACEMENT_3D ( 'NONE', #7812, #489, #14655 ) ;
#14950 = CARTESIAN_POINT ( 'NONE',  ( 58.72106816583844591, 13.02818770551464489, 16.17458954617363531 ) ) ;
#14951 = CARTESIAN_POINT ( 'NONE',  ( -2.117863837641485618E-16, 3.458734125000000326, 0.4875000013655952369 ) ) ;
#14952 = CARTESIAN_POINT ( 'NONE',  ( 3.458734125000001658, 1.432654583217640498, 15.25000000136560807 ) ) ;
#14953 = EDGE_CURVE ( 'NONE', #22213, #15687, #7057, .T. ) ;
#14954 = PLANE ( 'NONE',  #10732 ) ;
#14955 = CARTESIAN_POINT ( 'NONE',  ( -71.65000000109246514, 7.933012699999995476, 14.99999999999999645 ) ) ;
#14956 = EDGE_CURVE ( 'NONE', #22848, #4946, #22888, .T. ) ;
#14957 = CYLINDRICAL_SURFACE ( 'NONE', #16679, 11.00000000000000000 ) ;
#14958 = ORIENTED_EDGE ( 'NONE', *, *, #3194, .T. ) ;
#14959 = DIRECTION ( 'NONE',  ( 0.3420201433256622736, 0.9396926207859106484, 0.000000000000000000 ) ) ;
#14960 = LINE ( 'NONE', #4021, #21723 ) ;
#14961 = LINE ( 'NONE', #23555, #13224 ) ;
#14962 = ORIENTED_EDGE ( 'NONE', *, *, #14069, .T. ) ;
#14963 = ORIENTED_EDGE ( 'NONE', *, *, #11454, .T. ) ;
#14964 = CARTESIAN_POINT ( 'NONE',  ( 53.53125000000000000, 11.65685424949239923, 18.99999999999998934 ) ) ;
#14965 = ORIENTED_EDGE ( 'NONE', *, *, #20746, .T. ) ;
#14966 = CARTESIAN_POINT ( 'NONE',  ( 1.656854249492384135, -3.999999999999999112, 18.31250000000001421 ) ) ;
#14967 = VERTEX_POINT ( 'NONE', #3565 ) ;
#14968 = VECTOR ( 'NONE', #21183, 1000.000000000000000 ) ;
#14969 = AXIS2_PLACEMENT_3D ( 'NONE', #1565, #3599, #9146 ) ;
#14970 = CARTESIAN_POINT ( 'NONE',  ( 54.59606816583844591, 11.58880310854672935, 10.97181229448534445 ) ) ;
#14971 = MECHANICAL_DESIGN_GEOMETRIC_PRESENTATION_REPRESENTATION (  '', ( #13049 ), #9612 ) ;
#14972 = EDGE_CURVE ( 'NONE', #9225, #5230, #15286, .T. ) ;
#14973 = CARTESIAN_POINT ( 'NONE',  ( 65.40000000218495302, 9.999999999999998224, 17.49999999999999645 ) ) ;
#14974 = CARTESIAN_POINT ( 'NONE',  ( 66.09999999999999432, 9.999999999999998224, 17.49999999999999645 ) ) ;
#14975 = CARTESIAN_POINT ( 'NONE',  ( 71.80000000109245661, 9.143825827087050939, 12.93301269999999370 ) ) ;
#14976 = ADVANCED_FACE ( 'NONE', ( #2551 ), #13605, .T. ) ;
#14977 = EDGE_LOOP ( 'NONE', ( #12280, #18761, #3417, #15857 ) ) ;
#14978 = CARTESIAN_POINT ( 'NONE',  ( -3.999999999999999112, 1.656854249492380804, 18.06250000273119838 ) ) ;
#14979 = DIRECTION ( 'NONE',  ( -0.000000000000000000, -0.000000000000000000, 1.000000000000000000 ) ) ;
#14980 = CARTESIAN_POINT ( 'NONE',  ( 53.96643183416157541, 6.028187705514633343, 13.27509460956200016 ) ) ;
#14981 = CARTESIAN_POINT ( 'NONE',  ( 3.106864633348762617, -1.916927135885768907, 2.039999999999999147 ) ) ;
#14982 = EDGE_CURVE ( 'NONE', #15347, #9734, #2999, .T. ) ;
#14983 = CARTESIAN_POINT ( 'NONE',  ( 44.00000000000000711, -15.00000000000001954, 11.00000000000008882 ) ) ;
#14984 = VECTOR ( 'NONE', #16515, 1000.000000000000000 ) ;
#14985 = FACE_OUTER_BOUND ( 'NONE', #3167, .T. ) ;
#14986 = EDGE_CURVE ( 'NONE', #10654, #21424, #8906, .T. ) ;
#14987 = DIRECTION ( 'NONE',  ( 0.000000000000000000, 0.000000000000000000, 1.000000000000000000 ) ) ;
#14988 = CARTESIAN_POINT ( 'NONE',  ( -4.000000000000000000, 4.898587196589412829E-16, 19.04999999999996874 ) ) ;
#14989 = EDGE_LOOP ( 'NONE', ( #6775, #11122, #9287, #7256 ) ) ;
#14990 = CARTESIAN_POINT ( 'NONE',  ( -69.90000000218495302, 11.76776695296636888, 13.23223304703362579 ) ) ;
#14991 = CARTESIAN_POINT ( 'NONE',  ( 53.53125000000000000, 11.24264068711929276, 18.00000000000000000 ) ) ;
#14992 = CARTESIAN_POINT ( 'NONE',  ( 18.97172504071656363, -8.974600000000002353, 5.000000000000079936 ) ) ;
#14993 = EDGE_LOOP ( 'NONE', ( #10573, #17391, #20454, #16165 ) ) ;
#14994 = DIRECTION ( 'NONE',  ( 0.000000000000000000, 0.000000000000000000, 1.000000000000000000 ) ) ;
#14995 = CARTESIAN_POINT ( 'NONE',  ( 70.79999999999999716, 11.76776695296636888, 16.76776695296636532 ) ) ;
#14996 = DIRECTION ( 'NONE',  ( -1.000000000000000000, -7.703719777548943412E-32, 0.000000000000000000 ) ) ;
#14997 = CARTESIAN_POINT ( 'NONE',  ( 0.000000000000000000, 0.000000000000000000, -25.03750572909317285 ) ) ;
#14998 = ORIENTED_EDGE ( 'NONE', *, *, #23397, .F. ) ;
#14999 = CARTESIAN_POINT ( 'NONE',  ( -90.00000000000000000, 0.000000000000000000, 0.000000000000000000 ) ) ;
#15000 = VERTEX_POINT ( 'NONE', #12928 ) ;
#15001 = DIRECTION ( 'NONE',  ( 1.000000000000000000, -0.000000000000000000, -0.000000000000000000 ) ) ;
#15002 = CARTESIAN_POINT ( 'NONE',  ( -1.656854249492380138, -3.999999999999999112, 15.18750000000001066 ) ) ;
#15003 = DIRECTION ( 'NONE',  ( -1.000000000000000000, -0.000000000000000000, -0.000000000000000000 ) ) ;
#15004 = CARTESIAN_POINT ( 'NONE',  ( 4.197393957002303999, 7.772902908466098641E-14, -3.503767560748929810 ) ) ;
#15005 = DIRECTION ( 'NONE',  ( 0.9396926207859107594, -0.3420201433256623291, 3.697785493223492838E-32 ) ) ;
#15006 = CARTESIAN_POINT ( 'NONE',  ( 69.30000000109247082, 7.933012699999995476, 14.14382582708705094 ) ) ;
#15007 = ORIENTED_EDGE ( 'NONE', *, *, #6138, .F. ) ;
#15008 = CARTESIAN_POINT ( 'NONE',  ( 0.000000000000000000, 0.000000000000000000, -5.000000000000000888 ) ) ;
#15009 = EDGE_CURVE ( 'NONE', #11761, #15043, #4253, .T. ) ;
#15010 = CARTESIAN_POINT ( 'NONE',  ( 65.65000000109247935, 9.999999999999998224, 17.06698730000000097 ) ) ;
#15011 = CARTESIAN_POINT ( 'NONE',  ( 1.432654583217643163, -3.458734124999999437, 18.75000000136560274 ) ) ;
#15012 = LINE ( 'NONE', #20823, #21572 ) ;
#15013 = EDGE_CURVE ( 'NONE', #22188, #16763, #6287, .T. ) ;
#15014 = LINE ( 'NONE', #22268, #2328 ) ;
#15015 = CARTESIAN_POINT ( 'NONE',  ( 4.000000000000000888, -1.656854249492379694, 2.737500000000002043 ) ) ;
#15016 = CARTESIAN_POINT ( 'NONE',  ( -71.25000000218494733, 7.499999999999996447, 13.96446609406725514 ) ) ;
#15017 = CARTESIAN_POINT ( 'NONE',  ( -1.432654583217638944, 3.458734125000000326, 14.25000000136560629 ) ) ;
#15018 = DIRECTION ( 'NONE',  ( 0.000000000000000000, 0.000000000000000000, 1.000000000000000000 ) ) ;
#15019 = VERTEX_POINT ( 'NONE', #20988 ) ;
#15020 = CARTESIAN_POINT ( 'NONE',  ( -69.35000000109248219, 11.46158073645647235, 13.53841926354352232 ) ) ;
#15021 = EDGE_LOOP ( 'NONE', ( #15070, #2076 ) ) ;
#15022 = CARTESIAN_POINT ( 'NONE',  ( 52.27893183416158251, 8.411196891453236901, 10.97181229448535511 ) ) ;
#15023 = CARTESIAN_POINT ( 'NONE',  ( -71.40000000109246514, 10.85617417291294551, 17.06698729999999742 ) ) ;
#15024 = VERTEX_POINT ( 'NONE', #17070 ) ;
#15025 = CARTESIAN_POINT ( 'NONE',  ( 0.000000000000000000, -10.90201369670497655, -1.464956435139657343 ) ) ;
#15026 = ORIENTED_EDGE ( 'NONE', *, *, #1001, .T. ) ;
#15027 = VERTEX_POINT ( 'NONE', #17430 ) ;
#15028 = CARTESIAN_POINT ( 'NONE',  ( 1.432654583217643163, -3.458734124999999882, 18.00000000136560274 ) ) ;
#15029 = CARTESIAN_POINT ( 'NONE',  ( 52.78125000000000711, 8.757359312880703683, 11.99999999999999822 ) ) ;
#15030 = CARTESIAN_POINT ( 'NONE',  ( -68.05000000109247082, 9.999999999999998224, 17.06698730000000097 ) ) ;
#15031 = CARTESIAN_POINT ( 'NONE',  ( 69.00000000109247367, 7.933012699999995476, 15.85617417291294196 ) ) ;
#15032 = CARTESIAN_POINT ( 'NONE',  ( -67.00000000109247367, 9.143825827087050939, 12.93301269999999370 ) ) ;
#15033 = CARTESIAN_POINT ( 'NONE',  ( -3.458734124999999437, 1.432654583217640498, 11.62500000136560629 ) ) ;
#15034 = DIRECTION ( 'NONE',  ( 1.224646799147353207E-16, -0.000000000000000000, 1.000000000000000000 ) ) ;
#15035 = CARTESIAN_POINT ( 'NONE',  ( 57.81018183416157541, 12.99999999999999822, 15.06805114094562192 ) ) ;
#15036 = LINE ( 'NONE', #16569, #23061 ) ;
#15037 = CARTESIAN_POINT ( 'NONE',  ( 55.59375000000000711, 11.24264068711927322, 11.99999999999998934 ) ) ;
#15038 = LINE ( 'NONE', #748, #10141 ) ;
#15039 = CARTESIAN_POINT ( 'NONE',  ( -2.828427124746189403, 2.828427124746190291, 16.00000000273119838 ) ) ;
#15040 = CARTESIAN_POINT ( 'NONE',  ( 9.920644283265380691E-16, 4.000000000000000000, 10.75000000000001066 ) ) ;
#15041 = ORIENTED_EDGE ( 'NONE', *, *, #19346, .F. ) ;
#15042 = CARTESIAN_POINT ( 'NONE',  ( 0.000000000000000000, 0.000000000000000000, 9.480888224575631185 ) ) ;
#15043 = VERTEX_POINT ( 'NONE', #4125 ) ;
#15044 = CARTESIAN_POINT ( 'NONE',  ( 56.21643183416158251, 12.97181229448535689, 16.31069182806490758 ) ) ;
#15045 =( LENGTH_UNIT ( ) NAMED_UNIT ( * ) SI_UNIT ( .MILLI., .METRE. ) );
#15046 = CARTESIAN_POINT ( 'NONE',  ( -2.445694354108820523, 2.445694354108820523, 5.612500001365596347 ) ) ;
#15047 = PRODUCT_RELATED_PRODUCT_CATEGORY ( 'part', '', ( #13756 ) ) ;
#15048 = CONICAL_SURFACE ( 'NONE', #11211, 4.000000000000000000, 0.8911886515913786111 ) ;
#15049 = AXIS2_PLACEMENT_3D ( 'NONE', #5518, #7098, #21804 ) ;
#15050 = DIRECTION ( 'NONE',  ( -0.000000000000000000, -0.000000000000000000, 1.000000000000000000 ) ) ;
#15051 = VERTEX_POINT ( 'NONE', #16952 ) ;
#15052 = CARTESIAN_POINT ( 'NONE',  ( 9.920644283265380691E-16, 4.000000000000000000, 11.75000000000001066 ) ) ;
#15053 = EDGE_CURVE ( 'NONE', #15024, #23683, #18853, .T. ) ;
#15054 = CARTESIAN_POINT ( 'NONE',  ( 2.000000000000001776, 0.000000000000000000, 0.000000000000000000 ) ) ;
#15055 = CARTESIAN_POINT ( 'NONE',  ( -1.656854249492379472, 4.000000000000000000, 14.81250000000000888 ) ) ;
#15056 = ORIENTED_EDGE ( 'NONE', *, *, #15403, .T. ) ;
#15057 = CARTESIAN_POINT ( 'NONE',  ( -69.35000000218495586, 11.03553390593273598, 17.50000000000000355 ) ) ;
#15058 = CARTESIAN_POINT ( 'NONE',  ( -3.458734125000000770, 1.432654583217640498, -0.07499999863440427739 ) ) ;
#15059 = CARTESIAN_POINT ( 'NONE',  ( 68.09999999999999432, 9.999999999999998224, 12.49999999999999289 ) ) ;
#15060 = VECTOR ( 'NONE', #11180, 1000.000000000000000 ) ;
#15061 = CARTESIAN_POINT ( 'NONE',  ( 1.971781867644420635E-15, -4.000000000000000000, 11.25000000000001066 ) ) ;
#15062 = CARTESIAN_POINT ( 'NONE',  ( 4.999999999999999112, 0.000000000000000000, 0.000000000000000000 ) ) ;
#15063 = CARTESIAN_POINT ( 'NONE',  ( 51.12731816583844591, 12.87654654797634102, 17.78030770151602979 ) ) ;
#15064 = VECTOR ( 'NONE', #4671, 1000.000000000000000 ) ;
#15065 = CARTESIAN_POINT ( 'NONE',  ( -1.432654583217640276, 3.458734125000000326, -2.449999998634404097 ) ) ;
#15066 = CARTESIAN_POINT ( 'NONE',  ( 3.458734125000002546, -1.432654583217639610, 13.12500000136560629 ) ) ;
#15067 = LINE ( 'NONE', #13031, #9575 ) ;
#15068 = CARTESIAN_POINT ( 'NONE',  ( -72.00000000109248788, 12.06698729999999919, 14.14382582708705094 ) ) ;
#15069 = CARTESIAN_POINT ( 'NONE',  ( -70.04999999999999716, 11.03553390593273420, 17.50000000000000711 ) ) ;
#15070 = ORIENTED_EDGE ( 'NONE', *, *, #12133, .F. ) ;
#15071 = CARTESIAN_POINT ( 'NONE',  ( 72.50000000000000000, 9.999999999999998224, 14.99999999999999645 ) ) ;
#15072 = FACE_OUTER_BOUND ( 'NONE', #9086, .T. ) ;
#15073 = CARTESIAN_POINT ( 'NONE',  ( -70.20000000109246230, 12.06698730000000275, 14.14382582708705094 ) ) ;
#15074 = ORIENTED_EDGE ( 'NONE', *, *, #4567, .F. ) ;
#15075 = ORIENTED_EDGE ( 'NONE', *, *, #7365, .F. ) ;
#15076 = EDGE_CURVE ( 'NONE', #6397, #8139, #14339, .T. ) ;
#15077 = CARTESIAN_POINT ( 'NONE',  ( 0.000000000000000000, -2.357898499370432166, 3.035766082959412415E-15 ) ) ;
#15078 = EDGE_CURVE ( 'NONE', #23515, #701, #1849, .T. ) ;
#15079 = DIRECTION ( 'NONE',  ( 0.3420201433256622736, -0.9396926207859106484, -1.232595164407828100E-31 ) ) ;
#15080 = ORIENTED_EDGE ( 'NONE', *, *, #5123, .T. ) ;
#15081 = LINE ( 'NONE', #22337, #325 ) ;
#15082 = ORIENTED_EDGE ( 'NONE', *, *, #20606, .F. ) ;
#15083 = VECTOR ( 'NONE', #22678, 1000.000000000000000 ) ;
#15084 = CARTESIAN_POINT ( 'NONE',  ( 56.00231816583843170, 12.78030770151603868, 12.12345345202365188 ) ) ;
#15085 = EDGE_CURVE ( 'NONE', #17303, #8531, #23630, .T. ) ;
#15086 = CARTESIAN_POINT ( 'NONE',  ( 71.00000000109247367, 12.06698730000000275, 14.14382582708705094 ) ) ;
#15087 = CARTESIAN_POINT ( 'NONE',  ( 66.24999999999998579, 7.499999999999996447, 16.03553390593273775 ) ) ;
#15088 = CARTESIAN_POINT ( 'NONE',  ( 72.00000000109245946, 12.06698730000000275, 14.14382582708705094 ) ) ;
#15089 = PRODUCT_DEFINITION_SHAPE ( 'NONE', 'NONE',  #23718 ) ;
#15090 = ORIENTED_EDGE ( 'NONE', *, *, #11992, .T. ) ;
#15091 = CARTESIAN_POINT ( 'NONE',  ( 1.971781867644420635E-15, -4.000000000000000000, 15.37500000273119660 ) ) ;
#15092 = LINE ( 'NONE', #18885, #9545 ) ;
#15093 = CARTESIAN_POINT ( 'NONE',  ( 59.43750000000000711, 10.00000000000001776, 18.99999999999999645 ) ) ;
#15094 = FACE_OUTER_BOUND ( 'NONE', #6782, .T. ) ;
#15095 = DIRECTION ( 'NONE',  ( 0.000000000000000000, 0.000000000000000000, 1.000000000000000000 ) ) ;
#15096 = FACE_OUTER_BOUND ( 'NONE', #20341, .T. ) ;
#15097 = CARTESIAN_POINT ( 'NONE',  ( -65.90000000109247935, 9.143825827087049163, 17.06698730000000097 ) ) ;
#15098 = CARTESIAN_POINT ( 'NONE',  ( 0.000000000000000000, -6.478011392632939014, 6.807171995660559638 ) ) ;
#15099 = VERTEX_POINT ( 'NONE', #18745 ) ;
#15100 = DIRECTION ( 'NONE',  ( -1.000000000000000000, -7.703719777548943412E-32, 0.000000000000000000 ) ) ;
#15101 = ADVANCED_FACE ( 'NONE', ( #22796 ), #6408, .T. ) ;
#15102 = ORIENTED_EDGE ( 'NONE', *, *, #19737, .T. ) ;
#15103 = CARTESIAN_POINT ( 'NONE',  ( 4.101954839143060028, 2.368264730582927857, -3.681130640444267854 ) ) ;
#15104 = CARTESIAN_POINT ( 'NONE',  ( 70.59999999999999432, 11.76776695296636888, 13.23223304703362579 ) ) ;
#15105 = DIRECTION ( 'NONE',  ( 0.000000000000000000, 0.000000000000000000, -1.000000000000000000 ) ) ;
#15106 = EDGE_CURVE ( 'NONE', #4939, #10125, #2329, .T. ) ;
#15107 = CARTESIAN_POINT ( 'NONE',  ( -3.999999999999999112, 0.000000000000000000, 16.12500000273119838 ) ) ;
#15108 = VERTEX_POINT ( 'NONE', #20755 ) ;
#15109 = DIRECTION ( 'NONE',  ( -0.000000000000000000, -0.000000000000000000, -1.000000000000000000 ) ) ;
#15110 = ORIENTED_EDGE ( 'NONE', *, *, #11830, .F. ) ;
#15111 = CARTESIAN_POINT ( 'NONE',  ( -2.828427124746188515, -2.828427124746190735, 14.12500000000001066 ) ) ;
#15112 = ADVANCED_FACE ( 'NONE', ( #4362 ), #20978, .T. ) ;
#15113 = DIRECTION ( 'NONE',  ( 0.000000000000000000, 0.000000000000000000, 1.000000000000000000 ) ) ;
#15114 = EDGE_CURVE ( 'NONE', #10854, #17331, #21730, .T. ) ;
#15115 = CARTESIAN_POINT ( 'NONE',  ( 6.500000000000000888, 1.277696550142690457, -3.643982548855206449 ) ) ;
#15116 = CARTESIAN_POINT ( 'NONE',  ( 3.869372803233808611, -9.000000000000001776, 5.000000000000079936 ) ) ;
#15117 = CARTESIAN_POINT ( 'NONE',  ( 70.25000000109245946, 9.999999999999998224, 12.93301269999999192 ) ) ;
#15118 = EDGE_LOOP ( 'NONE', ( #8207, #12541, #1308 ) ) ;
#15119 = LINE ( 'NONE', #13197, #20226 ) ;
#15120 = CARTESIAN_POINT ( 'NONE',  ( 2.435583919667260400, -11.25000000000000355, 10.00000000000008882 ) ) ;
#15121 = CARTESIAN_POINT ( 'NONE',  ( 67.00000000109247367, 12.06698730000000275, 14.14382582708705094 ) ) ;
#15122 = CARTESIAN_POINT ( 'NONE',  ( -3.458734124999998993, 0.000000000000000000, 14.43750000136560452 ) ) ;
#15123 = CARTESIAN_POINT ( 'NONE',  ( 0.000000000000000000, 0.000000000000000000, -4.484454397937119197 ) ) ;
#15124 = AXIS2_PLACEMENT_3D ( 'NONE', #2778, #19194, #7958 ) ;
#15125 = CARTESIAN_POINT ( 'NONE',  ( 4.000000000000000000, 2.309401076758497151, -5.000000000000000000 ) ) ;
#15126 = CARTESIAN_POINT ( 'NONE',  ( -1.656854249492380804, 4.000000000000000000, 0.1125000000000017791 ) ) ;
#15127 = DIRECTION ( 'NONE',  ( -1.000000000000000000, -7.703719777548943412E-32, 0.000000000000000000 ) ) ;
#15128 = AXIS2_PLACEMENT_3D ( 'NONE', #21800, #7452, #18564 ) ;
#15129 = CARTESIAN_POINT ( 'NONE',  ( -3.458734124999998993, 0.000000000000000000, 15.43750000136560452 ) ) ;
#15130 = CARTESIAN_POINT ( 'NONE',  ( -67.40000000218495302, 9.999999999999998224, 12.49999999999999289 ) ) ;
#15131 = ORIENTED_EDGE ( 'NONE', *, *, #1593, .T. ) ;
#15132 = CARTESIAN_POINT ( 'NONE',  ( 4.000000000000000888, 1.656854249492381248, 15.68750000273119660 ) ) ;
#15133 = VERTEX_POINT ( 'NONE', #8457 ) ;
#15134 = CARTESIAN_POINT ( 'NONE',  ( 58.96875000000000711, 5.999999999999987566, 13.34314575050763452 ) ) ;
#15135 = CARTESIAN_POINT ( 'NONE',  ( -71.50000000109247367, 9.143825827087049163, 17.06698729999999742 ) ) ;
#15136 = ORIENTED_EDGE ( 'NONE', *, *, #11791, .T. ) ;
#15137 = PLANE ( 'NONE',  #15534 ) ;
#15138 = ORIENTED_EDGE ( 'NONE', *, *, #3835, .T. ) ;
#15139 = EDGE_CURVE ( 'NONE', #16212, #2919, #21104, .T. ) ;
#15140 = ORIENTED_EDGE ( 'NONE', *, *, #14377, .F. ) ;
#15141 = CARTESIAN_POINT ( 'NONE',  ( -1.432654583217639166, 3.458734125000000770, 18.50000000136560629 ) ) ;
#15142 = EDGE_CURVE ( 'NONE', #17845, #2131, #3390, .T. ) ;
#15143 = CARTESIAN_POINT ( 'NONE',  ( 56.71875000000000711, 13.00000000000000711, 16.24264068711927322 ) ) ;
#15144 = EDGE_CURVE ( 'NONE', #669, #21201, #10313, .T. ) ;
#15145 = VECTOR ( 'NONE', #6487, 1000.000000000000000 ) ;
#15146 = CARTESIAN_POINT ( 'NONE',  ( -66.40000000109247935, 10.85617417291294551, 17.06698729999999742 ) ) ;
#15147 = VECTOR ( 'NONE', #13417, 1000.000000000000000 ) ;
#15148 = CARTESIAN_POINT ( 'NONE',  ( 69.95000000109247651, 8.538419263543524096, 13.53841926354352054 ) ) ;
#15149 = CARTESIAN_POINT ( 'NONE',  ( -66.10000000109246798, 7.933012699999995476, 14.14382582708705094 ) ) ;
#15150 = CARTESIAN_POINT ( 'NONE',  ( 1.520000000000000462, 0.000000000000000000, -8.239200000000002078 ) ) ;
#15151 = CARTESIAN_POINT ( 'NONE',  ( 56.40393183416158251, 13.02818770551463778, 13.82541045382633982 ) ) ;
#15152 = DIRECTION ( 'NONE',  ( 1.000000000000000000, 0.000000000000000000, 0.000000000000000000 ) ) ;
#15153 = CARTESIAN_POINT ( 'NONE',  ( -1.432654583217641164, -3.458734125000000326, 3.175000001365598568 ) ) ;
#15154 = CARTESIAN_POINT ( 'NONE',  ( -2.445694354108818303, -2.445694354108820523, 11.56250000136560629 ) ) ;
#15155 = CARTESIAN_POINT ( 'NONE',  ( -2.828427124746188515, -2.828427124746190735, 14.25000000273119660 ) ) ;
#15156 = CARTESIAN_POINT ( 'NONE',  ( -69.05000000218494449, 11.03553390593276262, 12.50000000000001776 ) ) ;
#15157 = ORIENTED_EDGE ( 'NONE', *, *, #18126, .F. ) ;
#15158 = LINE ( 'NONE', #22778, #10919 ) ;
#15159 = ORIENTED_EDGE ( 'NONE', *, *, #18738, .F. ) ;
#15160 = CARTESIAN_POINT ( 'NONE',  ( 55.46643183416158962, 7.028187705514638672, 13.68930817193508531 ) ) ;
#15161 = CIRCLE ( 'NONE', #20463, 11.00000000000000000 ) ;
#15162 =( LENGTH_UNIT ( ) NAMED_UNIT ( * ) SI_UNIT ( .MILLI., .METRE. ) );
#15163 = CARTESIAN_POINT ( 'NONE',  ( -3.458734125000000326, 1.432654583217640276, 2.675000001365597679 ) ) ;
#15164 = CIRCLE ( 'NONE', #12500, 4.000000000000001776 ) ;
#15165 = CYLINDRICAL_SURFACE ( 'NONE', #18557, 4.000000000000001776 ) ;
#15166 = EDGE_LOOP ( 'NONE', ( #3641, #1926, #6248, #807 ) ) ;
#15167 = CARTESIAN_POINT ( 'NONE',  ( 9.920644283265380691E-16, 4.000000000000000000, 12.75000000000001066 ) ) ;
#15168 = CARTESIAN_POINT ( 'NONE',  ( 55.00000000000000711, -15.00000000000000000, 20.00000000000001421 ) ) ;
#15169 = ADVANCED_FACE ( 'NONE', ( #4719 ), #22918, .F. ) ;
#15170 = CARTESIAN_POINT ( 'NONE',  ( -20.00000000000001066, -10.00000000000000000, -49.99999999999999289 ) ) ;
#15171 = ORIENTED_EDGE ( 'NONE', *, *, #13250, .F. ) ;
#15172 = AXIS2_PLACEMENT_3D ( 'NONE', #22484, #17001, #21036 ) ;
#15173 = AXIS2_PLACEMENT_3D ( 'NONE', #10423, #3437, #10778 ) ;
#15174 = DIRECTION ( 'NONE',  ( 0.000000000000000000, 0.000000000000000000, 1.000000000000000000 ) ) ;
#15175 = CARTESIAN_POINT ( 'NONE',  ( 3.458734125000000770, 4.235727675282972223E-16, -1.512499998634402987 ) ) ;
#15176 = CARTESIAN_POINT ( 'NONE',  ( -5.969670414742686226, -4.058962678540103397, -3.296219944818621350 ) ) ;
#15177 = CARTESIAN_POINT ( 'NONE',  ( 68.54999999999999716, 8.964466094067258695, 17.50000000000000355 ) ) ;
#15178 = DIRECTION ( 'NONE',  ( -1.000000000000000000, 0.000000000000000000, -0.000000000000000000 ) ) ;
#15179 = CARTESIAN_POINT ( 'NONE',  ( -67.24999999999998579, 8.964466094067294222, 12.49999999999996092 ) ) ;
#15180 = CARTESIAN_POINT ( 'NONE',  ( 55.72106816583844591, 13.02818770551464489, 16.17458954617363531 ) ) ;
#15181 = CARTESIAN_POINT ( 'NONE',  ( 6.353591512924457348E-16, -3.458734125000000326, -2.012499998634403653 ) ) ;
#15182 = CARTESIAN_POINT ( 'NONE',  ( -3.458734124999998993, -1.432654583217642497, 15.75000000136560629 ) ) ;
#15183 = FACE_OUTER_BOUND ( 'NONE', #2522, .T. ) ;
#15184 = CARTESIAN_POINT ( 'NONE',  ( -70.65000000109246514, 9.999999999999998224, 17.06698730000000097 ) ) ;
#15185 = FACE_BOUND ( 'NONE', #18024, .T. ) ;
#15186 = ORIENTED_EDGE ( 'NONE', *, *, #14982, .F. ) ;
#15187 = CARTESIAN_POINT ( 'NONE',  ( -0.5469614295416921346, 4.303013824936271270, -3.535263753543735454 ) ) ;
#15188 = CARTESIAN_POINT ( 'NONE',  ( -1.656854249492380804, 4.000000000000000000, 4.237500002731185766 ) ) ;
#15189 = CARTESIAN_POINT ( 'NONE',  ( -70.60000000109246798, 7.933012699999995476, 15.85617417291294196 ) ) ;
#15190 = ORIENTED_EDGE ( 'NONE', *, *, #8560, .F. ) ;
#15191 = ORIENTED_EDGE ( 'NONE', *, *, #14217, .F. ) ;
#15192 = LINE ( 'NONE', #18511, #11020 ) ;
#15193 = DIRECTION ( 'NONE',  ( 0.000000000000000000, 0.000000000000000000, -1.000000000000000000 ) ) ;
#15194 = EDGE_LOOP ( 'NONE', ( #17608, #6552, #1094, #6273 ) ) ;
#15195 = FACE_OUTER_BOUND ( 'NONE', #8907, .T. ) ;
#15196 = CARTESIAN_POINT ( 'NONE',  ( 65.50000000218494733, 8.232233047033627571, 16.76776695296636532 ) ) ;
#15197 = CARTESIAN_POINT ( 'NONE',  ( -1.656854249492379250, 4.000000000000000000, 19.81250000000001776 ) ) ;
#15198 = CARTESIAN_POINT ( 'NONE',  ( 69.90000000109246514, 9.143825827087049163, 17.06698729999999742 ) ) ;
#15199 = ORIENTED_EDGE ( 'NONE', *, *, #12185, .T. ) ;
#15200 = CARTESIAN_POINT ( 'NONE',  ( -3.999999999999999112, 0.000000000000000000, 12.12500000273119838 ) ) ;
#15201 = EDGE_CURVE ( 'NONE', #5914, #2701, #6462, .T. ) ;
#15202 = AXIS2_PLACEMENT_3D ( 'NONE', #21469, #21350, #14085 ) ;
#15203 = CARTESIAN_POINT ( 'NONE',  ( 0.000000000000000000, 0.000000000000000000, -3.700000000000000178 ) ) ;
#15204 = CARTESIAN_POINT ( 'NONE',  ( 52.09143183416158251, 11.72490539043799984, 11.02818770551463246 ) ) ;
#15205 = CARTESIAN_POINT ( 'NONE',  ( 50.00000000000000000, 10.00000000000001599, 15.00000000000003020 ) ) ;
#15206 = CARTESIAN_POINT ( 'NONE',  ( 3.458734125000001214, 4.235727675282971730E-16, 16.93750000136560629 ) ) ;
#15207 = DIRECTION ( 'NONE',  ( 1.000000000000000000, 7.703719777548943412E-32, 0.000000000000000000 ) ) ;
#15208 = CARTESIAN_POINT ( 'NONE',  ( -66.20000000109246230, 9.143825827087052716, 12.93301269999999192 ) ) ;
#15209 = ORIENTED_EDGE ( 'NONE', *, *, #4977, .T. ) ;
#15210 = CARTESIAN_POINT ( 'NONE',  ( 35.00000000000000000, 7.500000000000001776, -20.00000000000000355 ) ) ;
#15211 = ORIENTED_EDGE ( 'NONE', *, *, #6310, .F. ) ;
#15212 = FACE_OUTER_BOUND ( 'NONE', #6857, .T. ) ;
#15213 = DIRECTION ( 'NONE',  ( 1.000000000000000000, 7.703719777548943412E-32, 0.000000000000000000 ) ) ;
#15214 = EDGE_CURVE ( 'NONE', #2635, #10924, #1226, .T. ) ;
#15215 = CIRCLE ( 'NONE', #2991, 11.00000000000000000 ) ;
#15216 = AXIS2_PLACEMENT_3D ( 'NONE', #12521, #3612, #21925 ) ;
#15217 = VERTEX_POINT ( 'NONE', #8809 ) ;
#15218 = CARTESIAN_POINT ( 'NONE',  ( 25.00005080000000035, 3.872983346207417021, 1.000000000000000000 ) ) ;
#15219 = DIRECTION ( 'NONE',  ( -1.000000000000000000, -0.000000000000000000, -0.000000000000000000 ) ) ;
#15220 = FACE_OUTER_BOUND ( 'NONE', #12064, .T. ) ;
#15221 = ORIENTED_EDGE ( 'NONE', *, *, #2346, .T. ) ;
#15222 = CARTESIAN_POINT ( 'NONE',  ( 1.656854249492380138, 4.000000000000000000, 0.9875000000000007105 ) ) ;
#15223 = VERTEX_POINT ( 'NONE', #23269 ) ;
#15224 = CARTESIAN_POINT ( 'NONE',  ( -13.27237933033274153, -11.25000000000000355, 5.000000000000079936 ) ) ;
#15225 = CARTESIAN_POINT ( 'NONE',  ( 1.656854249492381470, 4.000000000000000000, 12.68750000000001243 ) ) ;
#15226 = LINE ( 'NONE', #4063, #21032 ) ;
#15227 = TOROIDAL_SURFACE ( 'NONE', #1398, 6.200000000000020606, 0.1999999999999997613 ) ;
#15228 = VERTEX_POINT ( 'NONE', #10735 ) ;
#15229 = DIRECTION ( 'NONE',  ( -1.000000000000000000, 0.000000000000000000, -0.000000000000000000 ) ) ;
#15230 = DIRECTION ( 'NONE',  ( 0.9396926207859107594, -0.3420201433256623291, 3.697785493223492838E-32 ) ) ;
#15231 = CARTESIAN_POINT ( 'NONE',  ( 72.00000000109248788, 12.06698729999999919, 14.14382582708705094 ) ) ;
#15232 = ORIENTED_EDGE ( 'NONE', *, *, #3903, .F. ) ;
#15233 = AXIS2_PLACEMENT_3D ( 'NONE', #23191, #14004, #12219 ) ;
#15234 = ADVANCED_FACE ( 'NONE', ( #2907 ), #23391, .T. ) ;
#15235 = CARTESIAN_POINT ( 'NONE',  ( 60.00000000000000711, -9.999999999999998224, 19.99999999999999645 ) ) ;
#15236 = EDGE_CURVE ( 'NONE', #4233, #22239, #22122, .T. ) ;
#15237 = DIRECTION ( 'NONE',  ( 1.000000000000000000, 0.000000000000000000, 0.000000000000000000 ) ) ;
#15238 = CARTESIAN_POINT ( 'NONE',  ( 68.75000000109245946, 11.46158073645647235, 13.53841926354352232 ) ) ;
#15239 = CARTESIAN_POINT ( 'NONE',  ( -3.458734124999998993, 1.432654583217640276, 12.37500000136560629 ) ) ;
#15240 = CARTESIAN_POINT ( 'NONE',  ( -7.000000000000000000, 8.572527594031473190E-16, 5.000000000000009770 ) ) ;
#15241 = CARTESIAN_POINT ( 'NONE',  ( 0.000000000000000000, 0.000000000000000000, 0.000000000000000000 ) ) ;
#15242 = CARTESIAN_POINT ( 'NONE',  ( -1.656854249492380804, 4.000000000000000000, 2.112500000000001599 ) ) ;
#15243 = LINE ( 'NONE', #6121, #15060 ) ;
#15244 = DIRECTION ( 'NONE',  ( 0.000000000000000000, -1.000000000000000000, -1.040834085586083783E-14 ) ) ;
#15245 = LINE ( 'NONE', #22513, #5759 ) ;
#15246 = EDGE_CURVE ( 'NONE', #13807, #12252, #6995, .T. ) ;
#15247 = ADVANCED_FACE ( 'NONE', ( #23035 ), #10493, .F. ) ;
#15248 = VERTEX_POINT ( 'NONE', #5070 ) ;
#15249 = CARTESIAN_POINT ( 'NONE',  ( 20.39626908033275043, -11.25000000000000355, 5.000000000000079936 ) ) ;
#15250 = ORIENTED_EDGE ( 'NONE', *, *, #14404, .T. ) ;
#15251 = CARTESIAN_POINT ( 'NONE',  ( 52.09143183416158251, 11.72490539043799984, 11.02818770551463246 ) ) ;
#15252 = CARTESIAN_POINT ( 'NONE',  ( -68.05000000109247082, 12.06698730000000097, 14.99999999999999645 ) ) ;
#15253 = APPLICATION_PROTOCOL_DEFINITION ( 'draft international standard', 'automotive_design', 1998, #2718 ) ;
#15254 = ORIENTED_EDGE ( 'NONE', *, *, #10137, .T. ) ;
#15255 = CARTESIAN_POINT ( 'NONE',  ( 0.000000000000000000, 0.000000000000000000, 0.000000000000000000 ) ) ;
#15256 = VERTEX_POINT ( 'NONE', #16107 ) ;
#15257 = AXIS2_PLACEMENT_3D ( 'NONE', #6283, #7847, #4003 ) ;
#15258 = VECTOR ( 'NONE', #3141, 1000.000000000000000 ) ;
#15259 = EDGE_LOOP ( 'NONE', ( #21448, #2488, #7198, #4561 ) ) ;
#15260 = CARTESIAN_POINT ( 'NONE',  ( 1.872352939448454495E-15, -3.458734125000000770, 17.93750000136560274 ) ) ;
#15261 = CARTESIAN_POINT ( 'NONE',  ( 57.18750000000000000, 9.999999999999989342, 11.99999999999999467 ) ) ;
#15262 = AXIS2_PLACEMENT_3D ( 'NONE', #9283, #38, #15152 ) ;
#15263 = CARTESIAN_POINT ( 'NONE',  ( -69.20000000109246230, 9.143825827087050939, 12.93301269999999370 ) ) ;
#15264 = CARTESIAN_POINT ( 'NONE',  ( 68.80000000109247082, 10.85617417291294551, 17.06698730000000097 ) ) ;
#15265 = CARTESIAN_POINT ( 'NONE',  ( -68.35000000109246798, 8.538419263543522320, 16.46158073645647235 ) ) ;
#15266 =( BOUNDED_CURVE ( )  B_SPLINE_CURVE ( 2, ( #13291, #6083, #10826, #330, #18101, #22353, #4287, #1681, #9025 ),
 .UNSPECIFIED., .F., .F. ) 
 B_SPLINE_CURVE_WITH_KNOTS ( ( 3, 2, 2, 2, 3 ),
 ( 0.5500000000000000444, 0.5625000000000000000, 0.5749999999999999556, 0.5875000000000000222, 0.5999999999999999778 ),
 .UNSPECIFIED. ) 
 CURVE ( )  GEOMETRIC_REPRESENTATION_ITEM ( )  RATIONAL_B_SPLINE_CURVE ( ( 1.000000000000000000, 0.9238795325112867385, 1.000000000000000000, 0.9238795325112867385, 1.000000000000000000, 0.9238795325112867385, 1.000000000000000000, 0.9238795325112867385, 1.000000000000000000 ) ) 
 REPRESENTATION_ITEM ( '' )  );
#15267 = ADVANCED_FACE ( 'NONE', ( #5187 ), #2074, .F. ) ;
#15268 = DIRECTION ( 'NONE',  ( 0.000000000000000000, 0.000000000000000000, -1.000000000000000000 ) ) ;
#15269 = CARTESIAN_POINT ( 'NONE',  ( 57.34143183416159673, 8.689308171935088865, 17.97181229448535689 ) ) ;
#15270 = FACE_OUTER_BOUND ( 'NONE', #22810, .T. ) ;
#15271 = AXIS2_PLACEMENT_3D ( 'NONE', #18631, #2217, #16852 ) ;
#15272 = CARTESIAN_POINT ( 'NONE',  ( 2.445694354108820079, 2.445694354108820523, 4.612500001365595459 ) ) ;
#15273 = CARTESIAN_POINT ( 'NONE',  ( 1.432654583217643163, -3.458734124999999437, 12.75000000136560629 ) ) ;
#15274 = CARTESIAN_POINT ( 'NONE',  ( 1.656854249492381470, 4.000000000000000000, 10.81250000273119660 ) ) ;
#15275 = LINE ( 'NONE', #1948, #19884 ) ;
#15276 = EDGE_CURVE ( 'NONE', #1974, #3346, #22017, .T. ) ;
#15277 = ORIENTED_EDGE ( 'NONE', *, *, #1504, .T. ) ;
#15278 = CARTESIAN_POINT ( 'NONE',  ( 65.40000000218495302, 9.999999999999998224, 17.49999999999999645 ) ) ;
#15279 = VERTEX_POINT ( 'NONE', #14762 ) ;
#15280 = CARTESIAN_POINT ( 'NONE',  ( 56.96643183416158251, 7.028187705514638672, 13.68930817193508531 ) ) ;
#15281 = CARTESIAN_POINT ( 'NONE',  ( -2.445694354108819635, -2.445694354108820523, 1.862500001365596347 ) ) ;
#15282 = AXIS2_PLACEMENT_3D ( 'NONE', #2175, #22411, #13348 ) ;
#15283 = CARTESIAN_POINT ( 'NONE',  ( -3.458734124999999882, -1.432654583217642275, -0.1999999986344043745 ) ) ;
#15284 = ORIENTED_EDGE ( 'NONE', *, *, #9687, .T. ) ;
#15285 = CARTESIAN_POINT ( 'NONE',  ( -2.828427124746188515, -2.828427124746190735, 15.12500000000001066 ) ) ;
#15286 = CIRCLE ( 'NONE', #7625, 4.000000000000001776 ) ;
#15287 = CARTESIAN_POINT ( 'NONE',  ( 67.40000000218495302, 9.999999999999998224, 12.49999999999999289 ) ) ;
#15288 = DIRECTION ( 'NONE',  ( -0.06805114094563445570, 0.7054675904022865707, 0.7054675904022728039 ) ) ;
#15289 = ORIENTED_EDGE ( 'NONE', *, *, #5858, .T. ) ;
#15290 = PRODUCT ( 'hex flange nut gradea_iso_ISO - 4161 - M5 - N', 'hex flange nut gradea_iso_ISO - 4161 - M5 - N', '', ( #2405 ) ) ;
#15291 = CARTESIAN_POINT ( 'NONE',  ( -69.95000000218493597, 12.50000000000000000, 13.96446609406725869 ) ) ;
#15292 = CIRCLE ( 'NONE', #12614, 5.000000000000011546 ) ;
#15293 = FACE_OUTER_BOUND ( 'NONE', #3947, .T. ) ;
#15294 = AXIS2_PLACEMENT_3D ( 'NONE', #14983, #1768, #16875 ) ;
#15295 = CARTESIAN_POINT ( 'NONE',  ( -1.656854249492380138, -3.999999999999999112, 15.18750000000001066 ) ) ;
#15296 = CARTESIAN_POINT ( 'NONE',  ( 66.15000000000000568, 8.964466094067258695, 17.50000000000000355 ) ) ;
#15297 = VECTOR ( 'NONE', #18446, 1000.000000000000000 ) ;
#15298 = CARTESIAN_POINT ( 'NONE',  ( -14.98018309676618998, -9.000000000000003553, 5.000000000000079936 ) ) ;
#15299 = CARTESIAN_POINT ( 'NONE',  ( 69.45000000109247651, 12.06698730000000097, 14.99999999999999645 ) ) ;
#15300 = CIRCLE ( 'NONE', #18709, 2.649999999999999467 ) ;
#15301 = CARTESIAN_POINT ( 'NONE',  ( -65.00000000000000000, 9.999999999999998224, 17.49999999999999645 ) ) ;
#15302 = CARTESIAN_POINT ( 'NONE',  ( 53.47106816583843880, 6.971812294485350670, 13.82541045382635403 ) ) ;
#15303 = CARTESIAN_POINT ( 'NONE',  ( -3.458734125000000770, 0.000000000000000000, 3.987500001365595015 ) ) ;
#15304 = CARTESIAN_POINT ( 'NONE',  ( 1.025207404391860050E-15, 3.458734125000000770, 16.43750000136560629 ) ) ;
#15305 = EDGE_CURVE ( 'NONE', #18254, #6932, #20103, .T. ) ;
#15306 = CARTESIAN_POINT ( 'NONE',  ( 4.999999999999999112, 4.729683950898977862, -7.360373001730867060 ) ) ;
#15307 = CARTESIAN_POINT ( 'NONE',  ( -72.20000000109246230, 10.85617417291294551, 17.06698730000000097 ) ) ;
#15308 = EDGE_CURVE ( 'NONE', #8748, #9405, #2260, .T. ) ;
#15309 = CARTESIAN_POINT ( 'NONE',  ( 65.60000000218495586, 7.499999999999996447, 14.99999999999999645 ) ) ;
#15310 = ORIENTED_EDGE ( 'NONE', *, *, #551, .F. ) ;
#15311 = CARTESIAN_POINT ( 'NONE',  ( -0.6640947660597427138, 4.471078309994878985, -3.602146406945963442 ) ) ;
#15312 = AXIS2_PLACEMENT_3D ( 'NONE', #18391, #5578, #1971 ) ;
#15313 = CARTESIAN_POINT ( 'NONE',  ( -2.449293598294706907E-16, 4.000000000000000000, 3.175000002731189319 ) ) ;
#15314 = CARTESIAN_POINT ( 'NONE',  ( -70.75000000109247367, 8.538419263543524096, 13.53841926354352054 ) ) ;
#15315 = ORIENTED_EDGE ( 'NONE', *, *, #12159, .T. ) ;
#15316 =( REPRESENTATION_RELATIONSHIP ('NONE','NONE', #8403, #10226 ) REPRESENTATION_RELATIONSHIP_WITH_TRANSFORMATION ( #3853 )SHAPE_REPRESENTATION_RELATIONSHIP( ) );
#15317 = ORIENTED_EDGE ( 'NONE', *, *, #22829, .T. ) ;
#15318 = CARTESIAN_POINT ( 'NONE',  ( 72.50000000000000000, 9.999999999999998224, 17.49999999999999645 ) ) ;
#15319 = CIRCLE ( 'NONE', #20224, 0.2000000000000000944 ) ;
#15320 = CARTESIAN_POINT ( 'NONE',  ( 12.67929489676620314, -9.000000000000005329, 5.000000000000079936 ) ) ;
#15321 = EDGE_LOOP ( 'NONE', ( #9601, #22901, #20628 ) ) ;
#15322 = CARTESIAN_POINT ( 'NONE',  ( 44.06356521511867896, -9.086974644262722833, 10.00151577544548509 ) ) ;
#15323 = VECTOR ( 'NONE', #9424, 1000.000000000000000 ) ;
#15324 = UNCERTAINTY_MEASURE_WITH_UNIT (LENGTH_MEASURE( 1.000000000000000082E-05 ), #9885, 'distance_accuracy_value', 'NONE');
#15325 = CARTESIAN_POINT ( 'NONE',  ( 68.85000000109248219, 9.999999999999998224, 17.06698730000000097 ) ) ;
#15326 = CIRCLE ( 'NONE', #16453, 2.500000000000000888 ) ;
#15327 = CARTESIAN_POINT ( 'NONE',  ( 67.40000000109247935, 10.85617417291294551, 17.06698729999999742 ) ) ;
#15328 = ORIENTED_EDGE ( 'NONE', *, *, #11754, .F. ) ;
#15329 = LINE ( 'NONE', #20432, #10327 ) ;
#15330 = CARTESIAN_POINT ( 'NONE',  ( 58.03125000000000711, 11.65685424949239923, 18.99999999999998934 ) ) ;
#15331 = CARTESIAN_POINT ( 'NONE',  ( 2.828427124746192067, -2.828427124746189847, 12.50000000273119838 ) ) ;
#15332 = CARTESIAN_POINT ( 'NONE',  ( -3.458734124999998105, 1.432654583217640276, 19.37500000136560629 ) ) ;
#15333 = CIRCLE ( 'NONE', #4985, 2.700000000000000622 ) ;
#15334 = DIRECTION ( 'NONE',  ( 0.000000000000000000, 0.000000000000000000, -1.000000000000000000 ) ) ;
#15335 = CARTESIAN_POINT ( 'NONE',  ( 4.999999999999999112, -4.057423117305452465, 8.475820894092962021 ) ) ;
#15336 = ORIENTED_EDGE ( 'NONE', *, *, #12738, .F. ) ;
#15337 = CARTESIAN_POINT ( 'NONE',  ( -27.50000000000000711, 1.500000000000003109, -33.66025403784446723 ) ) ;
#15338 = CARTESIAN_POINT ( 'NONE',  ( -10.13078668033273999, -11.25000000000000355, 5.000000000000079936 ) ) ;
#15339 = PLANE ( 'NONE',  #1220 ) ;
#15340 = VECTOR ( 'NONE', #1747, 1000.000000000000000 ) ;
#15341 = ORIENTED_EDGE ( 'NONE', *, *, #8978, .T. ) ;
#15342 = FACE_BOUND ( 'NONE', #20243, .T. ) ;
#15343 = CARTESIAN_POINT ( 'NONE',  ( 54.99999999999992895, 15.00000000000000000, 5.000000000000001776 ) ) ;
#15344 = CARTESIAN_POINT ( 'NONE',  ( 1.656854249492384135, -3.999999999999999112, 11.43750000273119660 ) ) ;
#15345 = VECTOR ( 'NONE', #2536, 1000.000000000000000 ) ;
#15346 = FACE_OUTER_BOUND ( 'NONE', #21538, .T. ) ;
#15347 = VERTEX_POINT ( 'NONE', #2023 ) ;
#15348 = DIRECTION ( 'NONE',  ( -1.000000000000000000, 0.000000000000000000, 0.000000000000000000 ) ) ;
#15349 = ORIENTED_EDGE ( 'NONE', *, *, #3689, .T. ) ;
#15350 = EDGE_CURVE ( 'NONE', #10073, #4715, #14884, .T. ) ;
#15351 = DIRECTION ( 'NONE',  ( -1.000000000000000000, 0.000000000000000000, 0.000000000000000000 ) ) ;
#15352 = CARTESIAN_POINT ( 'NONE',  ( 1.656854249492384135, -3.999999999999999112, 13.31250000000001243 ) ) ;
#15353 = CARTESIAN_POINT ( 'NONE',  ( 70.80000000218494449, 12.50000000000000000, 14.99999999999999645 ) ) ;
#15354 = FACE_OUTER_BOUND ( 'NONE', #7583, .T. ) ;
#15355 =( NAMED_UNIT ( * ) SI_UNIT ( $, .STERADIAN. ) SOLID_ANGLE_UNIT ( ) );
#15356 = CARTESIAN_POINT ( 'NONE',  ( 71.10000000109246798, 10.85617417291294551, 12.93301269999999192 ) ) ;
#15357 = EDGE_CURVE ( 'NONE', #15024, #8094, #305, .T. ) ;
#15358 = ORIENTED_EDGE ( 'NONE', *, *, #10108, .F. ) ;
#15359 = VECTOR ( 'NONE', #17744, 1000.000000000000000 ) ;
#15360 = CARTESIAN_POINT ( 'NONE',  ( 3.802871176606126280, 5.309964801958118485, -0.01372220897661548429 ) ) ;
#15361 = FACE_OUTER_BOUND ( 'NONE', #7044, .T. ) ;
#15362 = CARTESIAN_POINT ( 'NONE',  ( 70.00000000109247367, 7.933012699999995476, 15.85617417291294196 ) ) ;
#15363 = CARTESIAN_POINT ( 'NONE',  ( -2.445694354108818303, -2.445694354108820523, 14.56250000136560452 ) ) ;
#15364 = DIRECTION ( 'NONE',  ( 1.000000000000000000, 0.000000000000000000, 0.000000000000000000 ) ) ;
#15365 = CARTESIAN_POINT ( 'NONE',  ( -19.99999999999999645, -9.000000000000003553, 5.000000000000079936 ) ) ;
#15366 = EDGE_LOOP ( 'NONE', ( #757, #5631 ) ) ;
#15367 = CARTESIAN_POINT ( 'NONE',  ( 7.347880794884118750E-16, -4.000000000000000000, 0.5500000000000018208 ) ) ;
#15368 = FACE_OUTER_BOUND ( 'NONE', #8195, .T. ) ;
#15369 = CARTESIAN_POINT ( 'NONE',  ( -2.445694354108819191, 2.445694354108820523, 10.31250000136560629 ) ) ;
#15370 = CARTESIAN_POINT ( 'NONE',  ( 39.24582498033275613, -11.25000000000000355, 5.000000000000079936 ) ) ;
#15371 = ORIENTED_EDGE ( 'NONE', *, *, #4977, .F. ) ;
#15372 = CARTESIAN_POINT ( 'NONE',  ( -67.35000000109248219, 8.538419263543522320, 16.46158073645647235 ) ) ;
#15373 = ORIENTED_EDGE ( 'NONE', *, *, #2461, .F. ) ;
#15374 = CARTESIAN_POINT ( 'NONE',  ( 59.81250000000000711, 14.00000000000000000, 14.99999999999997691 ) ) ;
#15375 = CARTESIAN_POINT ( 'NONE',  ( -67.35000000109246798, 11.46158073645647235, 16.46158073645647235 ) ) ;
#15376 = CONTEXT_DEPENDENT_SHAPE_REPRESENTATION ( #128, #10132 ) ;
#15377 = VERTEX_POINT ( 'NONE', #11535 ) ;
#15378 = LINE ( 'NONE', #2407, #8275 ) ;
#15379 = ORIENTED_EDGE ( 'NONE', *, *, #3832, .F. ) ;
#15380 = VECTOR ( 'NONE', #14889, 1000.000000000000000 ) ;
#15381 = EDGE_CURVE ( 'NONE', #19956, #20461, #20342, .T. ) ;
#15382 = EDGE_CURVE ( 'NONE', #3756, #14716, #3768, .T. ) ;
#15383 = VERTEX_POINT ( 'NONE', #13317 ) ;
#15384 = CARTESIAN_POINT ( 'NONE',  ( -3.458734124999998993, -1.432654583217642497, 16.75000000136560629 ) ) ;
#15385 = CARTESIAN_POINT ( 'NONE',  ( 58.31250000000000000, 13.00000000000000000, 14.99999999999998757 ) ) ;
#15386 = CARTESIAN_POINT ( 'NONE',  ( -66.45000000109247651, 9.999999999999998224, 17.06698730000000097 ) ) ;
#15387 = CARTESIAN_POINT ( 'NONE',  ( 69.70000000109247651, 9.143825827087049163, 17.06698730000000097 ) ) ;
#15388 = EDGE_CURVE ( 'NONE', #15720, #15000, #22379, .T. ) ;
#15389 = CARTESIAN_POINT ( 'NONE',  ( -72.44999999999998863, 11.03553390593273598, 17.50000000000000355 ) ) ;
#15390 = DIRECTION ( 'NONE',  ( -1.000000000000000000, -0.000000000000000000, -0.000000000000000000 ) ) ;
#15391 = CARTESIAN_POINT ( 'NONE',  ( 56.68518183416157541, 10.06805114094562548, 11.99999999999999645 ) ) ;
#15392 = CARTESIAN_POINT ( 'NONE',  ( -27.50000000000000711, 7.500000000000001776, -31.01025403784447221 ) ) ;
#15393 = CARTESIAN_POINT ( 'NONE',  ( -2.445694354108819635, -2.445694354108820967, 4.112500001365594571 ) ) ;
#15394 = DIRECTION ( 'NONE',  ( -0.000000000000000000, 1.000000000000000000, -0.000000000000000000 ) ) ;
#15395 = CARTESIAN_POINT ( 'NONE',  ( -3.999999999999998224, -1.656854249492383246, 11.18750000273119660 ) ) ;
#15396 = CARTESIAN_POINT ( 'NONE',  ( 27.56832511966726784, -11.25000000000000355, 5.000000000000079936 ) ) ;
#15397 = ORIENTED_EDGE ( 'NONE', *, *, #12133, .T. ) ;
#15398 = DIRECTION ( 'NONE',  ( 1.000000000000000000, 7.703719777548943412E-32, 0.000000000000000000 ) ) ;
#15399 = ORIENTED_EDGE ( 'NONE', *, *, #20000, .F. ) ;
#15400 = CARTESIAN_POINT ( 'NONE',  ( 59.40393183416158251, 13.02818770551463778, 13.82541045382633982 ) ) ;
#15401 =( NAMED_UNIT ( * ) PLANE_ANGLE_UNIT ( ) SI_UNIT ( $, .RADIAN. ) );
#15402 = CARTESIAN_POINT ( 'NONE',  ( -1.432654583217640276, 3.458734125000000326, 0.5500000013655963471 ) ) ;
#15403 = EDGE_CURVE ( 'NONE', #23070, #4760, #18913, .T. ) ;
#15404 = CARTESIAN_POINT ( 'NONE',  ( 6.353591512924457348E-16, -3.458734125000000326, 0.9875000013655956810 ) ) ;
#15405 = VERTEX_POINT ( 'NONE', #7803 ) ;
#15406 = CARTESIAN_POINT ( 'NONE',  ( -1.656854249492379250, 4.000000000000000000, 11.81250000000001066 ) ) ;
#15407 = ADVANCED_FACE ( 'NONE', ( #20586 ), #11648, .F. ) ;
#15408 = CARTESIAN_POINT ( 'NONE',  ( 9.920644283265380691E-16, 4.000000000000000000, 14.75000000000000888 ) ) ;
#15409 = EDGE_LOOP ( 'NONE', ( #12415, #14459, #987, #12844 ) ) ;
#15410 = CARTESIAN_POINT ( 'NONE',  ( -70.70000000218495018, 11.76776695296636888, 13.23223304703362579 ) ) ;
#15411 =( BOUNDED_CURVE ( )  B_SPLINE_CURVE ( 2, ( #8342, #22690, #12066, #4736, #15309, #6185, #22809, #13973, #13862 ),
 .UNSPECIFIED., .F., .F. ) 
 B_SPLINE_CURVE_WITH_KNOTS ( ( 3, 2, 2, 2, 3 ),
 ( 0.9375000000000007772, 0.9531250000000005551, 0.9687500000000004441, 0.9843750000000002220, 1.000000000000000000 ),
 .UNSPECIFIED. ) 
 CURVE ( )  GEOMETRIC_REPRESENTATION_ITEM ( )  RATIONAL_B_SPLINE_CURVE ( ( 0.9999999999999962252, 0.9238795325112905132, 1.000000000000000000, 0.9238795325112867385, 1.000000000000000000, 0.9238795325112867385, 1.000000000000000000, 0.9238795325112867385, 1.000000000000000000 ) ) 
 REPRESENTATION_ITEM ( '' )  );
#15412 = EDGE_CURVE ( 'NONE', #5919, #2990, #5306, .T. ) ;
#15413 = CARTESIAN_POINT ( 'NONE',  ( -2.117863837641485618E-16, 3.458734125000000770, -3.262499998634402765 ) ) ;
#15414 = EDGE_CURVE ( 'NONE', #21201, #6989, #1422, .T. ) ;
#15415 = CARTESIAN_POINT ( 'NONE',  ( -4.000000000000000000, -2.309401076758512694, -3.433295621305382461 ) ) ;
#15416 = CARTESIAN_POINT ( 'NONE',  ( -2.445694354108818303, -2.445694354108820967, 18.81250000136560629 ) ) ;
#15417 = CARTESIAN_POINT ( 'NONE',  ( 2.500000000000000000, 1.178949249685217415, 2.041999999999998483 ) ) ;
#15418 = CARTESIAN_POINT ( 'NONE',  ( 69.55000000109247082, 11.46158073645647235, 16.46158073645647235 ) ) ;
#15419 = LINE ( 'NONE', #2912, #754 ) ;
#15420 = CARTESIAN_POINT ( 'NONE',  ( 55.25231816583843170, 7.926799079670502124, 17.16943976678978245 ) ) ;
#15421 = CARTESIAN_POINT ( 'NONE',  ( 6.353591512924457348E-16, -3.458734125000000326, -3.012499998634404541 ) ) ;
#15422 = CARTESIAN_POINT ( 'NONE',  ( -2.445694354108818303, -2.445694354108820967, 11.81250000136560629 ) ) ;
#15423 = TOROIDAL_SURFACE ( 'NONE', #1987, 8.800000000000022027, 0.2000000000000011768 ) ;
#15424 = CARTESIAN_POINT ( 'NONE',  ( 0.000000000000000000, 0.000000000000000000, -4.974599999999998801 ) ) ;
#15425 = CARTESIAN_POINT ( 'NONE',  ( -68.25000000109245946, 9.999999999999998224, 17.06698730000000097 ) ) ;
#15426 = CYLINDRICAL_SURFACE ( 'NONE', #6254, 1.000000000000002665 ) ;
#15427 = CARTESIAN_POINT ( 'NONE',  ( 4.000000000000000000, 1.656854249492381248, -2.137499999999998401 ) ) ;
#15428 = EDGE_LOOP ( 'NONE', ( #4491, #15810, #16386, #5360 ) ) ;
#15429 = CARTESIAN_POINT ( 'NONE',  ( -3.999999999999999112, 0.000000000000000000, 18.12500000273119483 ) ) ;
#15430 = CARTESIAN_POINT ( 'NONE',  ( 1.489200000000000079, 0.000000000000000000, -8.239200000000002078 ) ) ;
#15431 = CARTESIAN_POINT ( 'NONE',  ( -69.40000000109249356, 12.06698730000000275, 14.14382582708705094 ) ) ;
#15432 = ORIENTED_EDGE ( 'NONE', *, *, #15861, .T. ) ;
#15433 = VERTEX_POINT ( 'NONE', #22741 ) ;
#15434 = CARTESIAN_POINT ( 'NONE',  ( -15.00000000000001066, 10.00000000000000000, -49.99999999999999289 ) ) ;
#15435 = CYLINDRICAL_SURFACE ( 'NONE', #1426, 10.00000000000000178 ) ;
#15436 = EDGE_LOOP ( 'NONE', ( #18427, #4983 ) ) ;
#15437 = CARTESIAN_POINT ( 'NONE',  ( 3.455068668934414777, -2.624017327439094327, -3.316620875263732504 ) ) ;
#15438 = EDGE_CURVE ( 'NONE', #21630, #7680, #9611, .T. ) ;
#15439 = CARTESIAN_POINT ( 'NONE',  ( 67.20000000109247651, 10.85617417291294551, 17.06698729999999742 ) ) ;
#15440 = ADVANCED_FACE ( 'NONE', ( #17132 ), #11283, .T. ) ;
#15441 = CARTESIAN_POINT ( 'NONE',  ( 69.20000000109246230, 7.933012699999995476, 15.85617417291294196 ) ) ;
#15442 = ORIENTED_EDGE ( 'NONE', *, *, #9490, .F. ) ;
#15443 =( BOUNDED_CURVE ( )  B_SPLINE_CURVE ( 2, ( #13857, #21112, #15771, #13967, #21229, #4841, #12175, #19445, #14208 ),
 .UNSPECIFIED., .F., .F. ) 
 B_SPLINE_CURVE_WITH_KNOTS ( ( 3, 2, 2, 2, 3 ),
 ( 0.6250000000000005551, 0.6406250000000004441, 0.6562500000000003331, 0.6718750000000002220, 0.6875000000000001110 ),
 .UNSPECIFIED. ) 
 CURVE ( )  GEOMETRIC_REPRESENTATION_ITEM ( )  RATIONAL_B_SPLINE_CURVE ( ( 0.9999999999999973355, 0.9238795325112894030, 1.000000000000000000, 0.9238795325112867385, 1.000000000000000000, 0.9238795325112867385, 1.000000000000000000, 0.9238795325112861834, 1.000000000000000444 ) ) 
 REPRESENTATION_ITEM ( '' )  );
#15444 = DIRECTION ( 'NONE',  ( 0.000000000000000000, -0.3090169943749549453, 0.9510565162951511997 ) ) ;
#15445 = CARTESIAN_POINT ( 'NONE',  ( 55.50000000000000711, 12.82842712474617741, 12.17157287525379239 ) ) ;
#15446 = LINE ( 'NONE', #7776, #4252 ) ;
#15447 = CARTESIAN_POINT ( 'NONE',  ( 1.025207404391860050E-15, 3.458734125000000326, 17.18750000136560274 ) ) ;
#15448 = CARTESIAN_POINT ( 'NONE',  ( -4.898587196589412829E-16, 0.000000000000000000, -4.000000000000000000 ) ) ;
#15449 = DIRECTION ( 'NONE',  ( 0.000000000000000000, 0.000000000000000000, 1.000000000000000000 ) ) ;
#15450 = VERTEX_POINT ( 'NONE', #4310 ) ;
#15451 = FACE_OUTER_BOUND ( 'NONE', #15936, .T. ) ;
#15452 = DIRECTION ( 'NONE',  ( 0.000000000000000000, 0.000000000000000000, -1.000000000000000000 ) ) ;
#15453 = DIRECTION ( 'NONE',  ( 0.000000000000000000, 1.000000000000000000, 3.491481338843133355E-15 ) ) ;
#15454 = ORIENTED_EDGE ( 'NONE', *, *, #22334, .T. ) ;
#15455 = VECTOR ( 'NONE', #18856, 1000.000000000000000 ) ;
#15456 = DIRECTION ( 'NONE',  ( -1.000000000000000000, -7.703719777548943412E-32, 0.000000000000000000 ) ) ;
#15457 = FACE_OUTER_BOUND ( 'NONE', #15998, .T. ) ;
#15458 = DIRECTION ( 'NONE',  ( 0.000000000000000000, 0.000000000000000000, 1.000000000000000000 ) ) ;
#15459 = CARTESIAN_POINT ( 'NONE',  ( -19.99999999999999645, -9.000000000000003553, 5.000000000000079936 ) ) ;
#15460 = ORIENTED_EDGE ( 'NONE', *, *, #17642, .T. ) ;
#15461 = CARTESIAN_POINT ( 'NONE',  ( 5.969670414742682674, 4.058962678540098956, -3.296219944818626235 ) ) ;
#15462 = ORIENTED_EDGE ( 'NONE', *, *, #16016, .T. ) ;
#15463 = CYLINDRICAL_SURFACE ( 'NONE', #6440, 8.749000000000002331 ) ;
#15464 = CARTESIAN_POINT ( 'NONE',  ( -65.75000000109245946, 9.999999999999998224, 17.49999999999999645 ) ) ;
#15465 = CARTESIAN_POINT ( 'NONE',  ( 70.95000000218495018, 11.03553390593273598, 17.50000000000000355 ) ) ;
#15466 = LINE ( 'NONE', #10196, #8792 ) ;
#15467 = CARTESIAN_POINT ( 'NONE',  ( 39.24582498033275613, -11.25000000000000355, 5.000000000000079936 ) ) ;
#15468 = CARTESIAN_POINT ( 'NONE',  ( 66.85000000109246798, 7.933012699999995476, 14.99999999999999645 ) ) ;
#15469 = ORIENTED_EDGE ( 'NONE', *, *, #12057, .T. ) ;
#15470 = CIRCLE ( 'NONE', #10498, 0.03079999999999923077 ) ;
#15471 = CARTESIAN_POINT ( 'NONE',  ( 3.525817189091411397, 5.469921996229798467, 4.860839739976680053E-15 ) ) ;
#15472 = DIRECTION ( 'NONE',  ( -1.000000000000000000, 0.000000000000000000, 1.982541115402065110E-16 ) ) ;
#15473 = CARTESIAN_POINT ( 'NONE',  ( 69.75000000109245946, 11.46158073645647235, 16.46158073645647235 ) ) ;
#15474 = CARTESIAN_POINT ( 'NONE',  ( -1.432654583217639610, -3.458734124999999882, 11.62500000136560452 ) ) ;
#15475 = DIRECTION ( 'NONE',  ( -1.224646799147353207E-16, 0.000000000000000000, -1.000000000000000000 ) ) ;
#15476 = EDGE_CURVE ( 'NONE', #22278, #7710, #14513, .T. ) ;
#15477 = DIRECTION ( 'NONE',  ( 0.000000000000000000, 0.000000000000000000, -1.000000000000000000 ) ) ;
#15478 = ORIENTED_EDGE ( 'NONE', *, *, #18296, .F. ) ;
#15479 = CARTESIAN_POINT ( 'NONE',  ( -4.000000000000000000, -1.656854249492383246, 0.3625000000000019873 ) ) ;
#15480 = FACE_OUTER_BOUND ( 'NONE', #16087, .T. ) ;
#15481 = CARTESIAN_POINT ( 'NONE',  ( 0.000000000000000000, -4.472189673936728838, -8.264486777890155622 ) ) ;
#15482 = DIRECTION ( 'NONE',  ( -1.000000000000000000, -0.000000000000000000, -0.000000000000000000 ) ) ;
#15483 = PRODUCT_DEFINITION_SHAPE ( 'NONE', 'NONE',  #23709 ) ;
#15484 = EDGE_LOOP ( 'NONE', ( #21325, #6360, #13271, #20562, #12340, #22756, #12242, #8534, #5681, #4329, #15341, #337, #2565, #7017, #19460, #16236, #21809, #20772, #1870 ) ) ;
#15485 = CARTESIAN_POINT ( 'NONE',  ( -66.15000000109247935, 11.46158073645647235, 13.53841926354352232 ) ) ;
#15486 = EDGE_LOOP ( 'NONE', ( #18465, #18923, #1933, #7405 ) ) ;
#15487 = CARTESIAN_POINT ( 'NONE',  ( -68.15000000109246514, 11.46158073645647235, 16.46158073645647235 ) ) ;
#15488 = CONTEXT_DEPENDENT_SHAPE_REPRESENTATION ( #21074, #19087 ) ;
#15489 = ORIENTED_EDGE ( 'NONE', *, *, #6100, .T. ) ;
#15490 = CARTESIAN_POINT ( 'NONE',  ( 32.96263968033274949, -11.25000000000000355, 5.000000000000079936 ) ) ;
#15491 = ORIENTED_EDGE ( 'NONE', *, *, #137, .F. ) ;
#15492 = ORIENTED_EDGE ( 'NONE', *, *, #23101, .F. ) ;
#15493 = CARTESIAN_POINT ( 'NONE',  ( 3.458734125000001658, 4.235727675282972223E-16, 12.18750000136560629 ) ) ;
#15494 = VECTOR ( 'NONE', #13584, 1000.000000000000114 ) ;
#15495 = CARTESIAN_POINT ( 'NONE',  ( 52.68750000000000711, 9.999999999999989342, 11.99999999999999467 ) ) ;
#15496 = CARTESIAN_POINT ( 'NONE',  ( -67.75000000109247367, 11.46158073645647235, 13.53841926354352232 ) ) ;
#15497 = FACE_OUTER_BOUND ( 'NONE', #12882, .T. ) ;
#15498 = VECTOR ( 'NONE', #4111, 1000.000000000000114 ) ;
#15499 = CARTESIAN_POINT ( 'NONE',  ( -72.09999999999999432, 9.999999999999998224, 12.49999999999999289 ) ) ;
#15500 = DIRECTION ( 'NONE',  ( -0.9396926207859107594, -0.3420201433256623291, 1.540743955509804830E-32 ) ) ;
#15501 = CARTESIAN_POINT ( 'NONE',  ( 55.18518183416157541, 10.06805114094562548, 11.99999999999999645 ) ) ;
#15502 = CARTESIAN_POINT ( 'NONE',  ( 0.000000000000000000, -2.357898499370432166, 3.035766082959412415E-15 ) ) ;
#15503 = EDGE_CURVE ( 'NONE', #9402, #21784, #828, .T. ) ;
#15504 = CARTESIAN_POINT ( 'NONE',  ( -1.432654583217640498, 3.458734125000000770, 1.800000001365597235 ) ) ;
#15505 = EDGE_CURVE ( 'NONE', #19718, #18634, #6867, .T. ) ;
#15506 = DIRECTION ( 'NONE',  ( -1.000000000000000000, -0.000000000000000000, -0.000000000000000000 ) ) ;
#15507 = CARTESIAN_POINT ( 'NONE',  ( -2.828427124746189403, 2.828427124746190291, 10.00000000273119660 ) ) ;
#15508 = DIRECTION ( 'NONE',  ( 0.000000000000000000, 0.000000000000000000, 1.000000000000000000 ) ) ;
#15509 = EDGE_LOOP ( 'NONE', ( #837, #12576, #9290, #2221 ) ) ;
#15510 = CARTESIAN_POINT ( 'NONE',  ( 0.000000000000000000, 4.057423117305515525, -8.475820894092930047 ) ) ;
#15511 = VERTEX_POINT ( 'NONE', #6230 ) ;
#15512 = CARTESIAN_POINT ( 'NONE',  ( 58.18518183416157541, 10.06805114094562548, 11.99999999999999645 ) ) ;
#15513 = CARTESIAN_POINT ( 'NONE',  ( 0.000000000000000000, 0.000000000000000000, 0.000000000000000000 ) ) ;
#15514 = CARTESIAN_POINT ( 'NONE',  ( 1.432654583217642275, -3.458734124999999437, 0.05000000136559582670 ) ) ;
#15515 = EDGE_CURVE ( 'NONE', #8094, #19958, #15119, .T. ) ;
#15516 = CARTESIAN_POINT ( 'NONE',  ( 3.458734125000000326, 1.432654583217640498, -0.6999999986344048741 ) ) ;
#15517 = ORIENTED_EDGE ( 'NONE', *, *, #21132, .F. ) ;
#15518 = AXIS2_PLACEMENT_3D ( 'NONE', #12335, #5004, #17815 ) ;
#15519 = CARTESIAN_POINT ( 'NONE',  ( -1.600000000000004086, 0.000000000000000000, 0.000000000000000000 ) ) ;
#15520 = DIRECTION ( 'NONE',  ( -1.000000000000000000, -0.000000000000000000, -0.000000000000000000 ) ) ;
#15521 = CIRCLE ( 'NONE', #20824, 4.000000000000000888 ) ;
#15522 = ORIENTED_EDGE ( 'NONE', *, *, #15865, .F. ) ;
#15523 = AXIS2_PLACEMENT_3D ( 'NONE', #4075, #11411, #9724 ) ;
#15524 = CARTESIAN_POINT ( 'NONE',  ( -4.000000000000000000, 2.309401076758498483, -3.433295621305379353 ) ) ;
#15525 = VERTEX_POINT ( 'NONE', #477 ) ;
#15526 = CARTESIAN_POINT ( 'NONE',  ( 54.97106816583843880, 6.971812294485350670, 13.82541045382635403 ) ) ;
#15527 = LINE ( 'NONE', #22564, #22064 ) ;
#15528 = CARTESIAN_POINT ( 'NONE',  ( -4.350941807883113910, -4.993536075455430101, -3.633174458636617921 ) ) ;
#15529 = DIRECTION ( 'NONE',  ( -1.000000000000000000, 0.000000000000000000, 0.000000000000000000 ) ) ;
#15530 = EDGE_CURVE ( 'NONE', #4037, #11622, #5990, .T. ) ;
#15531 = CARTESIAN_POINT ( 'NONE',  ( 0.000000000000000000, 1.178949249685217415, 2.041999999999998483 ) ) ;
#15532 = CARTESIAN_POINT ( 'NONE',  ( 70.90000000109246514, 10.85617417291294551, 12.93301269999999370 ) ) ;
#15533 = EDGE_CURVE ( 'NONE', #9405, #8728, #4172, .T. ) ;
#15535 = CYLINDRICAL_SURFACE ( 'NONE', #2294, 8.749000000000002331 ) ;
#15534 = AXIS2_PLACEMENT_3D ( 'NONE', #7357, #9498, #134 ) ;
#15536 = CARTESIAN_POINT ( 'NONE',  ( 53.37731816583844591, 7.830560233210212218, 12.92679907967049679 ) ) ;
#15537 = EDGE_CURVE ( 'NONE', #12610, #13749, #1500, .T. ) ;
#15538 = CIRCLE ( 'NONE', #12081, 4.000000000000001776 ) ;
#15539 = CARTESIAN_POINT ( 'NONE',  ( -2.117863837641485618E-16, 3.458734125000000326, -2.512499998634404097 ) ) ;
#15540 = CARTESIAN_POINT ( 'NONE',  ( -6.259644161404860030E-16, -4.618802153517027165, -3.433295621305388234 ) ) ;
#15541 = CARTESIAN_POINT ( 'NONE',  ( 67.29999999999999716, 9.999999999999998224, 12.49999999999999289 ) ) ;
#15542 = CARTESIAN_POINT ( 'NONE',  ( -68.65000000109246514, 9.999999999999998224, 12.93301269999999192 ) ) ;
#15543 = CARTESIAN_POINT ( 'NONE',  ( 4.000000000000003553, -2.309401076758513138, -3.504271511726786859 ) ) ;
#15544 = CARTESIAN_POINT ( 'NONE',  ( -69.70000000000000284, 9.999999999999998224, 12.49999999999999289 ) ) ;
#15545 = EDGE_LOOP ( 'NONE', ( #13045, #11183, #22425, #19334 ) ) ;
#15546 = CARTESIAN_POINT ( 'NONE',  ( -3.999999999999998224, -1.656854249492383024, 14.06250000000001066 ) ) ;
#15547 = CARTESIAN_POINT ( 'NONE',  ( 4.000000000000000888, -1.656854249492379694, 2.862500002731188431 ) ) ;
#15548 = EDGE_CURVE ( 'NONE', #19360, #5511, #19374, .T. ) ;
#15549 = ORIENTED_EDGE ( 'NONE', *, *, #12945, .F. ) ;
#15550 = VECTOR ( 'NONE', #14996, 1000.000000000000000 ) ;
#15551 = EDGE_CURVE ( 'NONE', #19246, #14452, #1057, .T. ) ;
#15552 = ORIENTED_EDGE ( 'NONE', *, *, #8623, .F. ) ;
#15553 = AXIS2_PLACEMENT_3D ( 'NONE', #15338, #8141, #15452 ) ;
#15554 = DIRECTION ( 'NONE',  ( 1.000000000000000000, 0.000000000000000000, -1.224646799147353207E-16 ) ) ;
#15555 =( BOUNDED_SURFACE ( )  B_SPLINE_SURFACE ( 3, 2, ( 
 ( #7865, #11482, #9674 ),
 ( #540, #15187, #15311 ),
 ( #11715, #6304, #13393 ),
 ( #20660, #656, #13739 ),
 ( #18981, #4377, #4264 ),
 ( #11600, #22692, #7990 ) ),
 .UNSPECIFIED., .F., .F., .F. ) 
 B_SPLINE_SURFACE_WITH_KNOTS ( ( 4, 2, 4 ),
 ( 3, 3 ),
 ( 0.02032853247518125531, 0.02278863295364820865, 0.02524873343211516200 ),
 ( 0.000000000000000000, 1.000000000000000000 ),
 .UNSPECIFIED. ) 
 GEOMETRIC_REPRESENTATION_ITEM ( )  RATIONAL_B_SPLINE_SURFACE ( (
 ( 1.000000000000000000, 0.8047781615896836271, 1.000000000000000000),
 ( 1.000000000000000000, 0.8123767586289967202, 1.000000000000000000),
 ( 1.000000000000000000, 0.8190662415563443322, 1.000000000000000000),
 ( 1.000000000000000000, 0.8192361015669982205, 1.000000000000000000),
 ( 1.000000000000000000, 0.8126135807103181952, 1.000000000000000000),
 ( 1.000000000000000000, 0.8047712338318587788, 1.000000000000000000) ) ) 
 REPRESENTATION_ITEM ( '' )  SURFACE ( )  );
#15556 = CARTESIAN_POINT ( 'NONE',  ( 4.999999999999999112, -2.223716399045513548, -8.461683424509336859 ) ) ;
#15557 = ORIENTED_EDGE ( 'NONE', *, *, #14953, .T. ) ;
#15558 = CARTESIAN_POINT ( 'NONE',  ( 27.50000000000000000, 1.500000000000003109, -36.31025403784446581 ) ) ;
#15559 = CIRCLE ( 'NONE', #23559, 8.749000000000002331 ) ;
#15560 = CIRCLE ( 'NONE', #19717, 2.500000000000002220 ) ;
#15561 = CARTESIAN_POINT ( 'NONE',  ( 68.65000000109247935, 12.06698730000000097, 14.99999999999999645 ) ) ;
#15562 = CARTESIAN_POINT ( 'NONE',  ( 68.20000000109246230, 10.85617417291294551, 17.06698729999999742 ) ) ;
#15563 = EDGE_LOOP ( 'NONE', ( #16502, #17784 ) ) ;
#15564 = DIRECTION ( 'NONE',  ( 0.000000000000000000, 0.4999999999999992784, -0.8660254037844389297 ) ) ;
#15565 = CARTESIAN_POINT ( 'NONE',  ( 57.46875000000000711, 5.999999999999987566, 13.34314575050763452 ) ) ;
#15566 = EDGE_CURVE ( 'NONE', #20146, #19235, #14143, .T. ) ;
#15567 = CARTESIAN_POINT ( 'NONE',  ( 1.971781867644420635E-15, -4.000000000000000000, 12.37500000273119838 ) ) ;
#15568 = CARTESIAN_POINT ( 'NONE',  ( 51.00000000000000711, 12.82842712474617741, 12.17157287525379239 ) ) ;
#15569 = DIRECTION ( 'NONE',  ( -1.000000000000000000, 0.000000000000000000, 0.000000000000000000 ) ) ;
#15570 = DIRECTION ( 'NONE',  ( 1.000000000000000000, 0.000000000000000000, 0.000000000000000000 ) ) ;
#15571 = ORIENTED_EDGE ( 'NONE', *, *, #17861, .T. ) ;
#15572 = LINE ( 'NONE', #22836, #9219 ) ;
#15573 = ADVANCED_FACE ( 'NONE', ( #21162 ), #22908, .T. ) ;
#15574 = CARTESIAN_POINT ( 'NONE',  ( -15.59503895323380362, -9.000000000000003553, 5.000000000000079936 ) ) ;
#15575 = LINE ( 'NONE', #22838, #15790 ) ;
#15576 = EDGE_CURVE ( 'NONE', #3743, #3912, #15712, .T. ) ;
#15577 = ORIENTED_EDGE ( 'NONE', *, *, #13199, .T. ) ;
#15578 = PLANE ( 'NONE',  #18941 ) ;
#15579 = LINE ( 'NONE', #22843, #2613 ) ;
#15580 = CARTESIAN_POINT ( 'NONE',  ( 35.00000000000000000, 4.500000000000009770, -4.286263797015736496E-15 ) ) ;
#15581 = DIRECTION ( 'NONE',  ( -0.000000000000000000, -0.000000000000000000, -1.000000000000000000 ) ) ;
#15582 = ORIENTED_EDGE ( 'NONE', *, *, #19459, .F. ) ;
#15583 = CARTESIAN_POINT ( 'NONE',  ( 3.525817189091411841, 5.469921996229796690, -3.700000000000005063 ) ) ;
#15584 = ORIENTED_EDGE ( 'NONE', *, *, #23089, .T. ) ;
#15585 = CARTESIAN_POINT ( 'NONE',  ( -18.72738675928344065, -8.974600000000002353, 5.000000000000079936 ) ) ;
#15586 = CARTESIAN_POINT ( 'NONE',  ( 0.000000000000000000, 0.000000000000000000, 0.000000000000000000 ) ) ;
#15587 = DIRECTION ( 'NONE',  ( 0.000000000000000000, 0.000000000000000000, 1.000000000000000000 ) ) ;
#15588 = CARTESIAN_POINT ( 'NONE',  ( 0.000000000000000000, -1.699438267350307008, -9.241976615262174732 ) ) ;
#15589 = CARTESIAN_POINT ( 'NONE',  ( 67.70000000109247651, 7.933012699999995476, 14.14382582708705094 ) ) ;
#15590 = ORIENTED_EDGE ( 'NONE', *, *, #7596, .T. ) ;
#15591 = DIRECTION ( 'NONE',  ( 0.000000000000000000, 0.5000000000000011102, 0.8660254037844379305 ) ) ;
#15592 = CARTESIAN_POINT ( 'NONE',  ( 0.000000000000000000, 0.000000000000000000, 19.04999999999996874 ) ) ;
#15593 = CARTESIAN_POINT ( 'NONE',  ( 70.25000000109245946, 9.999999999999998224, 12.93301269999999192 ) ) ;
#15594 = CARTESIAN_POINT ( 'NONE',  ( 3.458734125000001214, 1.432654583217640498, 13.00000000136560452 ) ) ;
#15595 = CARTESIAN_POINT ( 'NONE',  ( 25.24566549676620397, -9.000000000000001776, 5.000000000000079936 ) ) ;
#15596 = VECTOR ( 'NONE', #7389, 1000.000000000000000 ) ;
#15597 = FACE_OUTER_BOUND ( 'NONE', #12126, .T. ) ;
#15598 = ORIENTED_EDGE ( 'NONE', *, *, #12762, .F. ) ;
#15599 = CARTESIAN_POINT ( 'NONE',  ( -27.50000000000000711, 4.500000000000001776, -33.66025403784446723 ) ) ;
#15600 = CARTESIAN_POINT ( 'NONE',  ( -16.41397198033274307, -11.25000000000000355, 5.000000000000079936 ) ) ;
#15601 = CARTESIAN_POINT ( 'NONE',  ( -1.432654583217638944, 3.458734125000000326, 10.25000000136560452 ) ) ;
#15602 = DIRECTION ( 'NONE',  ( -0.000000000000000000, -1.000000000000000000, -0.000000000000000000 ) ) ;
#15603 = EDGE_CURVE ( 'NONE', #20532, #11553, #17198, .T. ) ;
#15604 = ORIENTED_EDGE ( 'NONE', *, *, #1471, .F. ) ;
#15605 = CARTESIAN_POINT ( 'NONE',  ( -67.20000000109246230, 10.85617417291294551, 17.06698730000000097 ) ) ;
#15606 = EDGE_LOOP ( 'NONE', ( #4268, #21009, #16921, #8263, #1245 ) ) ;
#15607 = AXIS2_PLACEMENT_3D ( 'NONE', #19528, #3485, #12376 ) ;
#15608 = CARTESIAN_POINT ( 'NONE',  ( -66.45000000109246230, 12.06698730000000097, 14.99999999999999645 ) ) ;
#15609 = EDGE_LOOP ( 'NONE', ( #12810, #18966, #4445, #23410 ) ) ;
#15610 = DIRECTION ( 'NONE',  ( -0.000000000000000000, -0.000000000000000000, 1.000000000000000000 ) ) ;
#15611 = VERTEX_POINT ( 'NONE', #8515 ) ;
#15612 = VECTOR ( 'NONE', #14460, 1000.000000000000114 ) ;
#15613 = ORIENTED_EDGE ( 'NONE', *, *, #48, .F. ) ;
#15614 = CARTESIAN_POINT ( 'NONE',  ( 3.458734125000001658, 1.432654583217640498, 12.25000000136560452 ) ) ;
#15615 = CARTESIAN_POINT ( 'NONE',  ( 52.03124999999999289, 11.24264068711929276, 18.00000000000000355 ) ) ;
#15616 = PRESENTATION_LAYER_ASSIGNMENT (  '', '', ( #18641 ) ) ;
#15617 = AXIS2_PLACEMENT_3D ( 'NONE', #21263, #6934, #23442 ) ;
#15618 = CYLINDRICAL_SURFACE ( 'NONE', #22050, 8.265000000000021885 ) ;
#15619 = DIRECTION ( 'NONE',  ( 1.000000000000000000, 0.000000000000000000, 0.000000000000000000 ) ) ;
#15620 = CARTESIAN_POINT ( 'NONE',  ( -70.50000000000000000, 9.999999999999998224, 12.49999999999999289 ) ) ;
#15621 = FACE_OUTER_BOUND ( 'NONE', #3922, .T. ) ;
#15622 = CARTESIAN_POINT ( 'NONE',  ( 59.96643183416158251, 6.028187705514633343, 13.27509460956200016 ) ) ;
#15623 = FACE_OUTER_BOUND ( 'NONE', #5079, .T. ) ;
#15624 = VECTOR ( 'NONE', #2848, 1000.000000000000000 ) ;
#15625 = CARTESIAN_POINT ( 'NONE',  ( 2.445694354108820967, -2.445694354108820079, 3.362500001365597679 ) ) ;
#15626 = DIRECTION ( 'NONE',  ( -1.000000000000000000, -7.703719777548943412E-32, 0.000000000000000000 ) ) ;
#15627 = CARTESIAN_POINT ( 'NONE',  ( 1.656854249492384135, -3.999999999999999112, 12.43750000273119838 ) ) ;
#15628 = CARTESIAN_POINT ( 'NONE',  ( 0.000000000000000000, 0.000000000000000000, 4.000000000000000000 ) ) ;
#15629 = CIRCLE ( 'NONE', #3725, 8.073750000000021743 ) ;
#15630 = ORIENTED_EDGE ( 'NONE', *, *, #21459, .T. ) ;
#15631 = FACE_OUTER_BOUND ( 'NONE', #3410, .T. ) ;
#15632 = ORIENTED_EDGE ( 'NONE', *, *, #23575, .T. ) ;
#15633 = CARTESIAN_POINT ( 'NONE',  ( 53.02893183416157541, 11.17458954617365663, 18.02818770551464311 ) ) ;
#15634 = SURFACE_STYLE_USAGE ( .BOTH. , #4820 ) ;
#15635 = CARTESIAN_POINT ( 'NONE',  ( -3.458734125000000326, 1.432654583217640276, -1.324999998634403209 ) ) ;
#15636 = ORIENTED_EDGE ( 'NONE', *, *, #19475, .T. ) ;
#15637 = DIRECTION ( 'NONE',  ( 0.000000000000000000, 0.000000000000000000, -1.000000000000000000 ) ) ;
#15638 = VERTEX_POINT ( 'NONE', #12234 ) ;
#15639 = CARTESIAN_POINT ( 'NONE',  ( -3.999999999999999112, 1.656854249492380582, 19.93750000000001066 ) ) ;
#15640 = VERTEX_POINT ( 'NONE', #23203 ) ;
#15641 = CARTESIAN_POINT ( 'NONE',  ( 50.18981816583844591, 9.931948859054346102, 10.99999999999999467 ) ) ;
#15642 = EDGE_CURVE ( 'NONE', #13392, #22910, #11915, .T. ) ;
#15643 = CARTESIAN_POINT ( 'NONE',  ( -67.25000000218494733, 7.499999999999995559, 13.96446609406725692 ) ) ;
#15644 = CARTESIAN_POINT ( 'NONE',  ( -2.445694354108820523, 2.445694354108820523, -1.137499998634402765 ) ) ;
#15645 = AXIS2_PLACEMENT_3D ( 'NONE', #10866, #8952, #18253 ) ;
#15646 = VECTOR ( 'NONE', #17658, 1000.000000000000000 ) ;
#15647 = DIRECTION ( 'NONE',  ( -0.000000000000000000, -0.000000000000000000, 1.000000000000000000 ) ) ;
#15648 = CARTESIAN_POINT ( 'NONE',  ( 2.445694354108822299, -2.445694354108820079, 19.06250000136560629 ) ) ;
#15649 = CARTESIAN_POINT ( 'NONE',  ( 4.000000000000000888, 1.656854249492381248, 15.68750000273119660 ) ) ;
#15650 = EDGE_CURVE ( 'NONE', #21452, #19427, #11996, .T. ) ;
#15651 = DIRECTION ( 'NONE',  ( -1.000000000000000000, 0.000000000000000000, 0.000000000000000000 ) ) ;
#15652 = CARTESIAN_POINT ( 'NONE',  ( 70.05000000109247082, 9.999999999999998224, 12.93301269999999192 ) ) ;
#15653 = DIRECTION ( 'NONE',  ( -1.000000000000000000, 0.000000000000000000, -0.000000000000000000 ) ) ;
#15654 = CARTESIAN_POINT ( 'NONE',  ( 52.25231816583844591, 7.926799079670502124, 17.16943976678978245 ) ) ;
#15655 = CARTESIAN_POINT ( 'NONE',  ( 2.445694354108820079, 2.445694354108820523, 0.6125000013655953479 ) ) ;
#15656 = CARTESIAN_POINT ( 'NONE',  ( 3.333333333333335702, -2.694301256218268215, -3.300726591567084256 ) ) ;
#15657 = CARTESIAN_POINT ( 'NONE',  ( 15.00195451966726523, -11.25000000000000355, 5.000000000000079936 ) ) ;
#15658 = CARTESIAN_POINT ( 'NONE',  ( -70.00000000109247367, 7.933012699999995476, 15.85617417291294196 ) ) ;
#15659 = ORIENTED_EDGE ( 'NONE', *, *, #21792, .F. ) ;
#15660 = CARTESIAN_POINT ( 'NONE',  ( 50.00000000000000000, -14.82704866393690857, 20.85615788968264894 ) ) ;
#15661 = DIRECTION ( 'NONE',  ( -1.000000000000000000, 0.000000000000000000, 0.000000000000000000 ) ) ;
#15662 = ORIENTED_EDGE ( 'NONE', *, *, #17844, .T. ) ;
#15663 = CARTESIAN_POINT ( 'NONE',  ( 1.656854249492384135, -3.999999999999999112, 15.43750000273119660 ) ) ;
#15664 = CARTESIAN_POINT ( 'NONE',  ( -4.000000000000000000, -1.656854249492383246, 2.487500002731188431 ) ) ;
#15665 = VERTEX_POINT ( 'NONE', #17722 ) ;
#15666 = ORIENTED_EDGE ( 'NONE', *, *, #2891, .F. ) ;
#15667 = CARTESIAN_POINT ( 'NONE',  ( 4.000000000000000000, 4.898587196589412829E-16, 1.925000002731188209 ) ) ;
#15668 = CYLINDRICAL_SURFACE ( 'NONE', #306, 2.500000000000009326 ) ;
#15669 = EDGE_LOOP ( 'NONE', ( #5483, #18817, #21040, #16204, #1960, #17453, #17742, #4880, #13569, #8006, #16273, #8520, #3928, #18938, #21003, #13601, #23590, #20602, #20718, #4403, #19255, #9275, #5853, #14962, #17474, #15662, #1213, #15940, #22259, #10659, #18893, #8205, #1303, #9848, #6806, #21028, #15211, #13682, #14483, #21096, #1693, #4970, #436, #567, #23102, #10421, #4793, #23557, #22556, #19952, #2065, #21328, #12490, #14691, #21568, #3997, #17594, #3283, #5323, #20102, #11363, #5591, #638, #16972, #17883, #3788, #10784, #15136, #13460, #23142, #7842, #9937, #2515, #20976, #22307, #17307, #14279, #7540, #19836, #10247, #20305, #14246, #15775, #15131, #19278 ) ) ;
#15670 = CARTESIAN_POINT ( 'NONE',  ( -3.999999999999999112, 0.000000000000000000, 18.00000000000001066 ) ) ;
#15671 = EDGE_CURVE ( 'NONE', #22965, #11837, #18332, .T. ) ;
#15672 = ADVANCED_FACE ( 'NONE', ( #10081, #16047 ), #15926, .F. ) ;
#15673 = AXIS2_PLACEMENT_3D ( 'NONE', #13552, #10082, #20819 ) ;
#15674 = CARTESIAN_POINT ( 'NONE',  ( 68.20000000109246230, 7.933012699999995476, 15.85617417291294196 ) ) ;
#15675 = AXIS2_PLACEMENT_3D ( 'NONE', #1178, #19263, #3098 ) ;
#15676 = CARTESIAN_POINT ( 'NONE',  ( 66.80000000109247082, 7.933012699999995476, 15.85617417291294196 ) ) ;
#15677 = EDGE_CURVE ( 'NONE', #7761, #14838, #5021, .T. ) ;
#15678 = PRODUCT_DEFINITION_SHAPE ( 'NONE', 'NONE',  #10500 ) ;
#15679 = ORIENTED_EDGE ( 'NONE', *, *, #8976, .F. ) ;
#15680 = MECHANICAL_DESIGN_GEOMETRIC_PRESENTATION_REPRESENTATION (  '', ( #17639 ), #16480 ) ;
#15681 = DIRECTION ( 'NONE',  ( -1.000000000000000000, 0.000000000000000000, 0.000000000000000000 ) ) ;
#15682 = CARTESIAN_POINT ( 'NONE',  ( 56.43750000000000000, 10.00000000000001776, 18.99999999999999645 ) ) ;
#15683 = CARTESIAN_POINT ( 'NONE',  ( 2.445694354108820079, 2.445694354108820523, 3.362500001365597679 ) ) ;
#15684 = CARTESIAN_POINT ( 'NONE',  ( -1.432654583217638944, 3.458734125000000326, 19.25000000136560629 ) ) ;
#15685 = FACE_BOUND ( 'NONE', #9916, .T. ) ;
#15686 = DIRECTION ( 'NONE',  ( 0.000000000000000000, 0.000000000000000000, -1.000000000000000000 ) ) ;
#15687 = VERTEX_POINT ( 'NONE', #19613 ) ;
#15688 = CARTESIAN_POINT ( 'NONE',  ( 0.9413949561959079615, 0.3373062947069093709, -19.99999999999999645 ) ) ;
#15689 =( BOUNDED_SURFACE ( )  B_SPLINE_SURFACE ( 1, 2, ( 
 ( #4121, #4359, #876, #641, #2549, #9895, #16834, #4605, #11463, #22674, #16950, #13721, #20518, #17067, #9770, #13493, #18850, #7741, #22562, #7973, #413, #2326, #15410, #20641, #6404, #20985, #8212, #22432, #2437, #22313, #11697, #13256, #18967, #6285, #9659, #4250, #6044, #15291, #19088, #4474, #17190, #6170, #13372, #11941, #2683, #11815, #528, #22793, #19206, #15057, #11583, #10022, #768, #7849, #8100, #5927, #20867, #19553, #3147, #10134, #4717, #21454, #12526, #1342, #17428, #10491, #5183, #17772, #4954, #17885, #23264, #8678, #10614, #12401, #8804, #22915, #1461, #6528, #8455, #15978, #19666, #12161, #6755, #21102, #6874, #5068, #19787, #14068, #12048, #994, #8321, #15643, #14312, #21571, #19314, #15762, #14196, #3269, #16105, #2905, #23144, #23389, #6991, #8562, #13847, #10251, #12288, #6643, #17541, #1109, #23033, #13957, #15870, #21215, #4829, #21334, #19430, #3027, #10377, #17663, #1224, #2048, #7472, #3615, #18008, #5655, #16332, #19907, #3388 ),
 ( #12648, #23626, #12991, #7241, #14431, #14668, #11196, #10954, #12871, #20124, #10731, #21697, #14791, #5782, #18356, #1584, #3731, #22167, #11072, #21927, #18470, #16563, #1938, #3860, #20254, #9389, #16216, #16682, #23503, #1697, #9278, #254, #5424, #32, #5307, #141, #22038, #13110, #7362, #3509, #8923, #7116, #10844, #7589, #14908, #18120, #9041, #14557, #21822, #12760, #20014, #16452, #18232, #1815, #9164, #5538, #13573, #15263, #16926, #6255, #22650, #2168, #2526, #18827, #17283, #18586, #17041, #17160, #22532, #849, #5902, #9866, #19060, #740, #20611, #11312, #20843, #9635, #13226, #20369, #15030, #22765, #9507, #20728, #8183, #6377, #15496, #22284, #8073, #20492, #3976, #384, #4221, #13343, #618, #22408, #16804, #2413, #11558, #7716, #4094, #18942, #503, #9992, #11435, #4451, #18710, #6017, #2299, #6143, #7825, #7944, #15386, #15146, #9745, #13468, #4332, #11788, #2651, #11672, #19401, #19286, #17856, #15948, #1311, #17396, #12374, #1428, #8768 ) ),
 .UNSPECIFIED., .F., .F., .F. ) 
 B_SPLINE_SURFACE_WITH_KNOTS ( ( 2, 2 ),
 ( 3, 2, 2, 2, 2, 2, 2, 2, 2, 2, 2, 2, 2, 2, 2, 2, 2, 2, 2, 2, 2, 2, 2, 2, 2, 2, 2, 2, 2, 2, 2, 2, 2, 2, 2, 2, 2, 2, 2, 2, 2, 2, 2, 2, 2, 2, 2, 2, 2, 2, 2, 2, 2, 2, 2, 2, 2, 2, 2, 2, 2, 2, 2, 2, 3 ),
 ( 0.000000000000000000, 1.000000000000000000 ),
 ( 0.000000000000000000, 0.01562500000000000000, 0.03125000000000000000, 0.04687500000000000000, 0.06250000000000000000, 0.07812500000000000000, 0.09375000000000000000, 0.1093750000000000000, 0.1250000000000000000, 0.1406250000000000000, 0.1562500000000000000, 0.1718750000000000000, 0.1875000000000000000, 0.2031250000000000000, 0.2187500000000000000, 0.2343750000000000000, 0.2500000000000000000, 0.2656250000000000000, 0.2812500000000000000, 0.2968750000000000000, 0.3125000000000000000, 0.3281250000000000000, 0.3437500000000000000, 0.3593750000000000000, 0.3750000000000000000, 0.3906250000000000000, 0.4062500000000000000, 0.4218750000000000000, 0.4375000000000000000, 0.4531250000000000000, 0.4687500000000000000, 0.4843750000000000000, 0.5000000000000000000, 0.5156250000000000000, 0.5312500000000000000, 0.5468750000000000000, 0.5625000000000000000, 0.5781250000000000000, 0.5937500000000000000, 0.6093750000000000000, 0.6250000000000000000, 0.6406250000000000000, 0.6562500000000000000, 0.6718750000000000000, 0.6875000000000000000, 0.7031250000000000000, 0.7187500000000000000, 0.7343750000000000000, 0.7500000000000000000, 0.7656250000000000000, 0.7812500000000000000, 0.7968750000000000000, 0.8125000000000000000, 0.8281250000000000000, 0.8437500000000000000, 0.8593750000000000000, 0.8750000000000000000, 0.8906250000000000000, 0.9062500000000000000, 0.9218750000000000000, 0.9375000000000000000, 0.9531250000000000000, 0.9687500000000000000, 0.9843750000000000000, 1.000000000000000000 ),
 .UNSPECIFIED. ) 
 GEOMETRIC_REPRESENTATION_ITEM ( )  RATIONAL_B_SPLINE_SURFACE ( (
 ( 1.000000000000000000, 0.9238795325112867385, 1.000000000000000000, 0.9238795325112867385, 1.000000000000000000, 0.9238795325112867385, 1.000000000000000000, 0.9238795325112867385, 1.000000000000000000, 0.9238795325112867385, 1.000000000000000000, 0.9238795325112867385, 1.000000000000000000, 0.9238795325112867385, 1.000000000000000000, 0.9238795325112867385, 1.000000000000000000, 0.9238795325112867385, 1.000000000000000000, 0.9238795325112867385, 1.000000000000000000, 0.9238795325112867385, 1.000000000000000000, 0.9238795325112867385, 1.000000000000000000, 0.9238795325112867385, 1.000000000000000000, 0.9238795325112867385, 1.000000000000000000, 0.9238795325112867385, 1.000000000000000000, 0.9238795325112867385, 1.000000000000000000, 0.9238795325112867385, 1.000000000000000000, 0.9238795325112867385, 1.000000000000000000, 0.9238795325112867385, 1.000000000000000000, 0.9238795325112867385, 1.000000000000000000, 0.9238795325112867385, 1.000000000000000000, 0.9238795325112867385, 1.000000000000000000, 0.9238795325112867385, 1.000000000000000000, 0.9238795325112867385, 1.000000000000000000, 0.9238795325112867385, 1.000000000000000000, 0.9238795325112867385, 1.000000000000000000, 0.9238795325112867385, 1.000000000000000000, 0.9238795325112867385, 1.000000000000000000, 0.9238795325112867385, 1.000000000000000000, 0.9238795325112867385, 1.000000000000000000, 0.9238795325112867385, 1.000000000000000000, 0.9238795325112867385, 1.000000000000000000, 0.9238795325112867385, 1.000000000000000000, 0.9238795325112867385, 1.000000000000000000, 0.9238795325112867385, 1.000000000000000000, 0.9238795325112867385, 1.000000000000000000, 0.9238795325112867385, 1.000000000000000000, 0.9238795325112867385, 1.000000000000000000, 0.9238795325112867385, 1.000000000000000000, 0.9238795325112867385, 1.000000000000000000, 0.9238795325112867385, 1.000000000000000000, 0.9238795325112867385, 1.000000000000000000, 0.9238795325112867385, 1.000000000000000000, 0.9238795325112867385, 1.000000000000000000, 0.9238795325112867385, 1.000000000000000000, 0.9238795325112867385, 1.000000000000000000, 0.9238795325112867385, 1.000000000000000000, 0.9238795325112867385, 1.000000000000000000, 0.9238795325112867385, 1.000000000000000000, 0.9238795325112867385, 1.000000000000000000, 0.9238795325112867385, 1.000000000000000000, 0.9238795325112867385, 1.000000000000000000, 0.9238795325112867385, 1.000000000000000000, 0.9238795325112867385, 1.000000000000000000, 0.9238795325112867385, 1.000000000000000000, 0.9238795325112867385, 1.000000000000000000, 0.9238795325112867385, 1.000000000000000000, 0.9238795325112867385, 1.000000000000000000, 0.9238795325112867385, 1.000000000000000000, 0.9238795325112867385, 1.000000000000000000, 0.9238795325112867385, 1.000000000000000000, 0.9238795325112867385, 1.000000000000000000, 0.9238795325112867385, 1.000000000000000000, 0.9238795325112867385, 1.000000000000000000),
 ( 1.000000000000000000, 0.9238795325112867385, 1.000000000000000000, 0.9238795325112867385, 1.000000000000000000, 0.9238795325112867385, 1.000000000000000000, 0.9238795325112867385, 1.000000000000000000, 0.9238795325112867385, 1.000000000000000000, 0.9238795325112867385, 1.000000000000000000, 0.9238795325112867385, 1.000000000000000000, 0.9238795325112867385, 1.000000000000000000, 0.9238795325112867385, 1.000000000000000000, 0.9238795325112867385, 1.000000000000000000, 0.9238795325112867385, 1.000000000000000000, 0.9238795325112867385, 1.000000000000000000, 0.9238795325112867385, 1.000000000000000000, 0.9238795325112867385, 1.000000000000000000, 0.9238795325112867385, 1.000000000000000000, 0.9238795325112867385, 1.000000000000000000, 0.9238795325112867385, 1.000000000000000000, 0.9238795325112867385, 1.000000000000000000, 0.9238795325112867385, 1.000000000000000000, 0.9238795325112867385, 1.000000000000000000, 0.9238795325112867385, 1.000000000000000000, 0.9238795325112867385, 1.000000000000000000, 0.9238795325112867385, 1.000000000000000000, 0.9238795325112867385, 1.000000000000000000, 0.9238795325112867385, 1.000000000000000000, 0.9238795325112867385, 1.000000000000000000, 0.9238795325112867385, 1.000000000000000000, 0.9238795325112867385, 1.000000000000000000, 0.9238795325112867385, 1.000000000000000000, 0.9238795325112867385, 1.000000000000000000, 0.9238795325112867385, 1.000000000000000000, 0.9238795325112867385, 1.000000000000000000, 0.9238795325112867385, 1.000000000000000000, 0.9238795325112867385, 1.000000000000000000, 0.9238795325112867385, 1.000000000000000000, 0.9238795325112867385, 1.000000000000000000, 0.9238795325112867385, 1.000000000000000000, 0.9238795325112867385, 1.000000000000000000, 0.9238795325112867385, 1.000000000000000000, 0.9238795325112867385, 1.000000000000000000, 0.9238795325112867385, 1.000000000000000000, 0.9238795325112867385, 1.000000000000000000, 0.9238795325112867385, 1.000000000000000000, 0.9238795325112867385, 1.000000000000000000, 0.9238795325112867385, 1.000000000000000000, 0.9238795325112867385, 1.000000000000000000, 0.9238795325112867385, 1.000000000000000000, 0.9238795325112867385, 1.000000000000000000, 0.9238795325112867385, 1.000000000000000000, 0.9238795325112867385, 1.000000000000000000, 0.9238795325112867385, 1.000000000000000000, 0.9238795325112867385, 1.000000000000000000, 0.9238795325112867385, 1.000000000000000000, 0.9238795325112867385, 1.000000000000000000, 0.9238795325112867385, 1.000000000000000000, 0.9238795325112867385, 1.000000000000000000, 0.9238795325112867385, 1.000000000000000000, 0.9238795325112867385, 1.000000000000000000, 0.9238795325112867385, 1.000000000000000000, 0.9238795325112867385, 1.000000000000000000, 0.9238795325112867385, 1.000000000000000000, 0.9238795325112867385, 1.000000000000000000, 0.9238795325112867385, 1.000000000000000000, 0.9238795325112867385, 1.000000000000000000) ) ) 
 REPRESENTATION_ITEM ( '' )  SURFACE ( )  );
#15690 = LINE ( 'NONE', #18896, #18571 ) ;
#15691 = DIRECTION ( 'NONE',  ( 0.000000000000000000, 0.9510565162951544194, -0.3090169943749447312 ) ) ;
#15692 = ORIENTED_EDGE ( 'NONE', *, *, #1844, .T. ) ;
#15693 = VECTOR ( 'NONE', #21490, 1000.000000000000000 ) ;
#15694 = FACE_OUTER_BOUND ( 'NONE', #21748, .T. ) ;
#15695 = CARTESIAN_POINT ( 'NONE',  ( 4.000000000000001776, -1.656854249492379694, 11.56250000273119660 ) ) ;
#15696 = EDGE_CURVE ( 'NONE', #6665, #462, #16053, .T. ) ;
#15697 = DIRECTION ( 'NONE',  ( 0.000000000000000000, 0.000000000000000000, -1.000000000000000000 ) ) ;
#15698 = ORIENTED_EDGE ( 'NONE', *, *, #16710, .F. ) ;
#15699 = CARTESIAN_POINT ( 'NONE',  ( -9.302608809283439584, -8.974600000000002353, 10.00000000000008882 ) ) ;
#15700 = ORIENTED_EDGE ( 'NONE', *, *, #6365, .T. ) ;
#15701 = CARTESIAN_POINT ( 'NONE',  ( 71.40000000109249356, 7.933012699999995476, 15.85617417291294196 ) ) ;
#15702 = AXIS2_PLACEMENT_3D ( 'NONE', #3892, #16847, #7860 ) ;
#15703 = ADVANCED_FACE ( 'NONE', ( #17489 ), #17369, .F. ) ;
#15704 = CARTESIAN_POINT ( 'NONE',  ( -5.968343123267132455, 4.059728990630802059, -0.4033376246892508288 ) ) ;
#15705 = DIRECTION ( 'NONE',  ( 0.000000000000000000, 0.000000000000000000, -1.000000000000000000 ) ) ;
#15706 = CARTESIAN_POINT ( 'NONE',  ( 68.60000000109246798, 9.143825827087052716, 12.93301269999999192 ) ) ;
#15707 = EDGE_CURVE ( 'NONE', #7114, #7929, #1438, .T. ) ;
#15708 = ORIENTED_EDGE ( 'NONE', *, *, #11855, .F. ) ;
#15709 = AXIS2_PLACEMENT_3D ( 'NONE', #9998, #17287, #22770 ) ;
#15710 = EDGE_CURVE ( 'NONE', #6666, #23109, #6091, .T. ) ;
#15711 = VECTOR ( 'NONE', #4483, 1000.000000000000000 ) ;
#15712 = LINE ( 'NONE', #17610, #22531 ) ;
#15713 = CARTESIAN_POINT ( 'NONE',  ( -1.656854249492380138, -3.999999999999999112, 10.31250000273119660 ) ) ;
#15714 = CARTESIAN_POINT ( 'NONE',  ( 69.85000000109246798, 9.999999999999998224, 17.06698730000000097 ) ) ;
#15715 = CARTESIAN_POINT ( 'NONE',  ( 3.458734125000001214, 1.432654583217640498, 11.00000000136560452 ) ) ;
#15716 = VECTOR ( 'NONE', #21257, 1000.000000000000000 ) ;
#15717 = CARTESIAN_POINT ( 'NONE',  ( 5.200000000000002842, 0.000000000000000000, 0.000000000000000000 ) ) ;
#15718 = CYLINDRICAL_SURFACE ( 'NONE', #9631, 6.000000000000000888 ) ;
#15719 = AXIS2_PLACEMENT_3D ( 'NONE', #10940, #17869, #3370 ) ;
#15720 = VERTEX_POINT ( 'NONE', #14732 ) ;
#15721 = CARTESIAN_POINT ( 'NONE',  ( -2.828427124746189403, -2.828427124746190735, -2.574999999999999289 ) ) ;
#15722 = DIRECTION ( 'NONE',  ( -1.000000000000000000, -7.703719777548943412E-32, 0.000000000000000000 ) ) ;
#15723 = CARTESIAN_POINT ( 'NONE',  ( 118.3095189484530181, 15.00000000000001954, 10.00000000000008882 ) ) ;
#15724 = DIRECTION ( 'NONE',  ( -1.000000000000000000, 0.000000000000000000, 0.000000000000000000 ) ) ;
#15725 = VERTEX_POINT ( 'NONE', #1993 ) ;
#15726 = CARTESIAN_POINT ( 'NONE',  ( 4.000000000000000888, 4.898587196589412829E-16, 13.62500000273119660 ) ) ;
#15727 = ORIENTED_EDGE ( 'NONE', *, *, #12899, .F. ) ;
#15728 = CARTESIAN_POINT ( 'NONE',  ( -66.25000000109245946, 9.999999999999998224, 12.93301269999999192 ) ) ;
#15729 = CONTEXT_DEPENDENT_SHAPE_REPRESENTATION ( #7183, #722 ) ;
#15730 = EDGE_LOOP ( 'NONE', ( #11638, #17213, #897, #6059 ) ) ;
#15731 = CARTESIAN_POINT ( 'NONE',  ( -3.999999999999999112, 0.000000000000000000, 11.00000000000001066 ) ) ;
#15732 = ORIENTED_EDGE ( 'NONE', *, *, #6439, .F. ) ;
#15733 = ORIENTED_EDGE ( 'NONE', *, *, #16451, .T. ) ;
#15734 = CARTESIAN_POINT ( 'NONE',  ( 2.445694354108821411, 2.445694354108820523, 12.31250000136560629 ) ) ;
#15735 = CARTESIAN_POINT ( 'NONE',  ( 51.84375000000001421, 8.757359312880723223, 18.00000000000000355 ) ) ;
#15736 = AXIS2_PLACEMENT_3D ( 'NONE', #18439, #226, #22134 ) ;
#15737 = CARTESIAN_POINT ( 'NONE',  ( -19.99999999999999645, -15.00000000000001954, 5.000000000000079936 ) ) ;
#15738 = AXIS2_PLACEMENT_3D ( 'NONE', #17144, #7926, #15724 ) ;
#15739 = CARTESIAN_POINT ( 'NONE',  ( 67.25000000109247367, 9.999999999999998224, 17.06698730000000097 ) ) ;
#15740 = EDGE_CURVE ( 'NONE', #19075, #18380, #21751, .T. ) ;
#15741 = EDGE_CURVE ( 'NONE', #4177, #6681, #5485, .T. ) ;
#15742 = CARTESIAN_POINT ( 'NONE',  ( -69.74999999999998579, 11.03553390593273598, 12.49999999999999289 ) ) ;
#15743 = DIRECTION ( 'NONE',  ( 0.000000000000000000, 0.000000000000000000, 1.000000000000000000 ) ) ;
#15744 = CARTESIAN_POINT ( 'NONE',  ( 52.37268183416157541, 7.926799079670491466, 12.83056023321021755 ) ) ;
#15745 = CARTESIAN_POINT ( 'NONE',  ( 6.353591512924457348E-16, -3.458734125000000770, 0.2375000013655967357 ) ) ;
#15746 = CARTESIAN_POINT ( 'NONE',  ( 67.00000000218494733, 9.999999999999998224, 17.49999999999999645 ) ) ;
#15747 = CARTESIAN_POINT ( 'NONE',  ( 9.920644283265380691E-16, 4.000000000000000000, 10.87500000273119660 ) ) ;
#15748 = LINE ( 'NONE', #17295, #6523 ) ;
#15749 = AXIS2_PLACEMENT_3D ( 'NONE', #6118, #20825, #11889 ) ;
#15750 = ORIENTED_EDGE ( 'NONE', *, *, #13406, .T. ) ;
#15751 = CARTESIAN_POINT ( 'NONE',  ( 31.52885079676620705, -9.000000000000005329, 10.00000000000008882 ) ) ;
#15752 = VERTEX_POINT ( 'NONE', #14380 ) ;
#15753 = CARTESIAN_POINT ( 'NONE',  ( 54.62268183416157541, 12.07320092032950676, 17.16943976678977180 ) ) ;
#15754 = DIRECTION ( 'NONE',  ( -1.000000000000000000, 0.000000000000000000, 0.000000000000000000 ) ) ;
#15755 = VERTEX_POINT ( 'NONE', #17950 ) ;
#15756 = CARTESIAN_POINT ( 'NONE',  ( 0.000000000000000000, 0.000000000000000000, 0.000000000000000000 ) ) ;
#15757 = SHAPE_REPRESENTATION ( 'hex flange nut gradea_iso_ISO - 4161 - M5 - N', ( #7318 ), #16773 ) ;
#15758 = VERTEX_POINT ( 'NONE', #7184 ) ;
#15759 = FACE_OUTER_BOUND ( 'NONE', #14084, .T. ) ;
#15760 = ORIENTED_EDGE ( 'NONE', *, *, #12447, .T. ) ;
#15761 = CARTESIAN_POINT ( 'NONE',  ( 57.68981816583843170, 9.931948859054354983, 11.99999999999999645 ) ) ;
#15762 = CARTESIAN_POINT ( 'NONE',  ( -67.05000000218494449, 8.964466094067258695, 17.50000000000000355 ) ) ;
#15763 = CARTESIAN_POINT ( 'NONE',  ( -3.381512639161500466, 0.7267833367865139671, -3.295601554149589330 ) ) ;
#15764 = CARTESIAN_POINT ( 'NONE',  ( -72.15000000109246514, 11.46158073645647235, 16.46158073645647235 ) ) ;
#15765 = CARTESIAN_POINT ( 'NONE',  ( -3.458734124999999437, 1.432654583217640498, 17.62500000136560274 ) ) ;
#15766 = CARTESIAN_POINT ( 'NONE',  ( 2.828427124746192067, -2.828427124746189847, 13.50000000273119660 ) ) ;
#15767 = CARTESIAN_POINT ( 'NONE',  ( 58.12500000000000000, 12.12132034355964727, 17.12132034355963484 ) ) ;
#15768 = CARTESIAN_POINT ( 'NONE',  ( 71.10000000109246798, 12.06698730000000275, 15.85617417291294196 ) ) ;
#15769 = CARTESIAN_POINT ( 'NONE',  ( 59.62500000000000711, 12.12132034355964727, 17.12132034355963484 ) ) ;
#15770 = CARTESIAN_POINT ( 'NONE',  ( 2.445694354108820079, 2.445694354108820523, 2.612500001365597235 ) ) ;
#15771 = CARTESIAN_POINT ( 'NONE',  ( 67.70000000218493597, 11.76776695296636888, 16.76776695296636532 ) ) ;
#15772 = DIRECTION ( 'NONE',  ( 0.000000000000000000, 0.000000000000000000, 1.000000000000000000 ) ) ;
#15773 = CARTESIAN_POINT ( 'NONE',  ( -68.45000000109247651, 7.933012699999995476, 14.99999999999999645 ) ) ;
#15774 = EDGE_CURVE ( 'NONE', #2729, #19492, #14499, .T. ) ;
#15775 = ORIENTED_EDGE ( 'NONE', *, *, #16541, .F. ) ;
#15776 = DIRECTION ( 'NONE',  ( -1.000000000000000000, 0.000000000000000000, -0.000000000000000000 ) ) ;
#15777 = DIRECTION ( 'NONE',  ( 0.000000000000000000, 0.000000000000000000, 1.000000000000000000 ) ) ;
#15778 = ORIENTED_EDGE ( 'NONE', *, *, #16405, .F. ) ;
#15779 = CARTESIAN_POINT ( 'NONE',  ( 72.50000000000000000, 9.999999999999998224, 14.99999999999999645 ) ) ;
#15780 = CARTESIAN_POINT ( 'NONE',  ( -1.656854249492381248, -3.999999999999999112, 1.612500002731187543 ) ) ;
#15781 = ORIENTED_EDGE ( 'NONE', *, *, #12756, .F. ) ;
#15782 = ORIENTED_EDGE ( 'NONE', *, *, #2229, .T. ) ;
#15783 = CARTESIAN_POINT ( 'NONE',  ( 36.99310306966726358, -11.25000000000000355, 10.00000000000008882 ) ) ;
#15784 = DIRECTION ( 'NONE',  ( -0.000000000000000000, 0.000000000000000000, -1.000000000000000000 ) ) ;
#15785 = ORIENTED_EDGE ( 'NONE', *, *, #22805, .T. ) ;
#15786 = CARTESIAN_POINT ( 'NONE',  ( 3.453038570460273071, 2.625189405340834448, -3.535263753543585352 ) ) ;
#15787 = UNCERTAINTY_MEASURE_WITH_UNIT (LENGTH_MEASURE( 1.000000000000000082E-05 ), #16369, 'distance_accuracy_value', 'NONE');
#15788 = CARTESIAN_POINT ( 'NONE',  ( 66.70000000109246230, 7.933012699999995476, 14.14382582708705094 ) ) ;
#15789 = CARTESIAN_POINT ( 'NONE',  ( 69.15000000109246514, 8.538419263543522320, 16.46158073645647235 ) ) ;
#15790 = VECTOR ( 'NONE', #6452, 1000.000000000000000 ) ;
#15791 = CARTESIAN_POINT ( 'NONE',  ( -65.55000000218494449, 7.499999999999996447, 16.03553390593273775 ) ) ;
#15792 = CYLINDRICAL_SURFACE ( 'NONE', #8424, 4.000000000000000000 ) ;
#15793 = CARTESIAN_POINT ( 'NONE',  ( 55.25231816583843170, 7.219692298483957771, 17.87654654797633924 ) ) ;
#15794 = CARTESIAN_POINT ( 'NONE',  ( 1.432654583217639832, 3.458734125000000326, 2.425000001365597679 ) ) ;
#15795 = CARTESIAN_POINT ( 'NONE',  ( 1.872352939448454495E-15, -3.458734125000000326, 15.68750000136560629 ) ) ;
#15796 = DIRECTION ( 'NONE',  ( 0.000000000000000000, 0.000000000000000000, 1.000000000000000000 ) ) ;
#15797 = EDGE_CURVE ( 'NONE', #22762, #5267, #16166, .T. ) ;
#15798 = DIRECTION ( 'NONE',  ( -0.000000000000000000, -0.000000000000000000, 1.000000000000000000 ) ) ;
#15799 = ORIENTED_EDGE ( 'NONE', *, *, #16575, .T. ) ;
#15800 = DIRECTION ( 'NONE',  ( 0.000000000000000000, 0.000000000000000000, 1.000000000000000000 ) ) ;
#15801 = EDGE_CURVE ( 'NONE', #15108, #15051, #21641, .T. ) ;
#15802 = CARTESIAN_POINT ( 'NONE',  ( 72.37500000054622262, 9.999999999999998224, 17.28349365000000049 ) ) ;
#15803 = EDGE_LOOP ( 'NONE', ( #1756, #19142, #11265, #7781 ) ) ;
#15804 = CARTESIAN_POINT ( 'NONE',  ( -2.828427124746189403, 2.828427124746190291, 14.00000000273119660 ) ) ;
#15805 = CARTESIAN_POINT ( 'NONE',  ( 71.60000000109246798, 9.143825827087050939, 12.93301269999999370 ) ) ;
#15806 = EDGE_CURVE ( 'NONE', #17589, #2967, #5714, .T. ) ;
#15807 = LINE ( 'NONE', #5118, #1811 ) ;
#15808 = ORIENTED_EDGE ( 'NONE', *, *, #21664, .T. ) ;
#15809 = CARTESIAN_POINT ( 'NONE',  ( 4.999999999999999112, 0.000000000000000000, 8.749000000000002331 ) ) ;
#15810 = ORIENTED_EDGE ( 'NONE', *, *, #13185, .F. ) ;
#15811 = CARTESIAN_POINT ( 'NONE',  ( 53.34375000000000000, 8.343145750507638070, 19.00000000000000711 ) ) ;
#15812 = CARTESIAN_POINT ( 'NONE',  ( 71.00000000218494733, 9.999999999999998224, 17.49999999999999645 ) ) ;
#15813 = CARTESIAN_POINT ( 'NONE',  ( 27.50000000000000000, 1.500000000000003109, -36.31025403784446581 ) ) ;
#15814 = CARTESIAN_POINT ( 'NONE',  ( 50.00000000000000000, 2.399706452296379577, 55.00000000000021316 ) ) ;
#15815 = CARTESIAN_POINT ( 'NONE',  ( 65.90000000109247935, 9.143825827087049163, 17.06698730000000097 ) ) ;
#15816 = VERTEX_POINT ( 'NONE', #3678 ) ;
#15817 = DIRECTION ( 'NONE',  ( 0.000000000000000000, 0.000000000000000000, -1.000000000000000000 ) ) ;
#15818 = EDGE_CURVE ( 'NONE', #23109, #2045, #12467, .T. ) ;
#15819 = CARTESIAN_POINT ( 'NONE',  ( 7.347880794884118750E-16, -4.000000000000000000, -1.324999997268811347 ) ) ;
#15820 = CARTESIAN_POINT ( 'NONE',  ( 4.999999999999999112, -7.593217523260522128, -7.958834565716849774 ) ) ;
#15821 = CARTESIAN_POINT ( 'NONE',  ( 3.458734125000001658, 4.235727675282972223E-16, 19.18750000136560629 ) ) ;
#15822 = CARTESIAN_POINT ( 'NONE',  ( -2.000000000000000888, 7.592810154713614487E-16, 6.200000000000020606 ) ) ;
#15823 = DIRECTION ( 'NONE',  ( 0.3420201433256622736, 0.9396926207859106484, 0.000000000000000000 ) ) ;
#15824 = ORIENTED_EDGE ( 'NONE', *, *, #20956, .F. ) ;
#15825 = CARTESIAN_POINT ( 'NONE',  ( 4.000000000000000888, -1.656854249492379694, -1.262499999999997513 ) ) ;
#15826 = ADVANCED_FACE ( 'NONE', ( #12714 ), #18184, .T. ) ;
#15827 = LINE ( 'NONE', #8407, #17066 ) ;
#15828 = DIRECTION ( 'NONE',  ( 0.3420201433256622181, 0.9396926207859107594, -6.162975822039141593E-32 ) ) ;
#15829 = CARTESIAN_POINT ( 'NONE',  ( -72.09999999999999432, 9.999999999999998224, 12.49999999999999289 ) ) ;
#15830 = ORIENTED_EDGE ( 'NONE', *, *, #4095, .F. ) ;
#15831 = CARTESIAN_POINT ( 'NONE',  ( 72.50000000000000000, 9.999999999999998224, 14.99999999999999645 ) ) ;
#15832 = EDGE_LOOP ( 'NONE', ( #19834, #20241, #16214, #21895 ) ) ;
#15833 = CARTESIAN_POINT ( 'NONE',  ( -6.500000000000000000, 0.6345343291280529652, 5.374424050328533679E-16 ) ) ;
#15834 = ITEM_DEFINED_TRANSFORMATION ( 'NONE', 'NONE', #4953,  #7318 ) ;
#15835 = EDGE_CURVE ( 'NONE', #21232, #6397, #20993, .T. ) ;
#15836 = EDGE_LOOP ( 'NONE', ( #19305, #4269, #5988, #23255 ) ) ;
#15837 = DIRECTION ( 'NONE',  ( 0.000000000000000000, 0.000000000000000000, 1.000000000000000000 ) ) ;
#15838 = ORIENTED_EDGE ( 'NONE', *, *, #1502, .F. ) ;
#15839 = EDGE_CURVE ( 'NONE', #15665, #4019, #9945, .T. ) ;
#15840 = ORIENTED_EDGE ( 'NONE', *, *, #20365, .F. ) ;
#15841 = CARTESIAN_POINT ( 'NONE',  ( -2.445694354108818303, -2.445694354108820967, 12.81250000136560629 ) ) ;
#15842 = CARTESIAN_POINT ( 'NONE',  ( 4.999999999999999112, -8.734705317681630277, 0.4999240074894146790 ) ) ;
#15843 = VECTOR ( 'NONE', #4365, 1000.000000000000114 ) ;
#15844 = CARTESIAN_POINT ( 'NONE',  ( 0.000000000000000000, 1.178949249685212974, -2.042000000000001148 ) ) ;
#15845 = TOROIDAL_SURFACE ( 'NONE', #6653, 6.760799999999997034, 0.03079999999999879709 ) ;
#15846 = DIRECTION ( 'NONE',  ( 0.000000000000000000, -0.000000000000000000, -1.000000000000000000 ) ) ;
#15847 = CARTESIAN_POINT ( 'NONE',  ( -68.99999999999998579, 11.76776695296636888, 13.23223304703362579 ) ) ;
#15848 = CARTESIAN_POINT ( 'NONE',  ( 4.999999999999999112, -8.461683424509297780, -2.223716399045659653 ) ) ;
#15849 = CARTESIAN_POINT ( 'NONE',  ( 60.00000000000001421, 10.96484721591755473, 18.28038746411511184 ) ) ;
#15850 = CARTESIAN_POINT ( 'NONE',  ( 3.458734125000000770, 1.432654583217640498, -0.4499999986344046521 ) ) ;
#15851 = EDGE_CURVE ( 'NONE', #8889, #22700, #4283, .T. ) ;
#15852 = DIRECTION ( 'NONE',  ( 0.000000000000000000, 0.000000000000000000, 1.000000000000000000 ) ) ;
#15853 = CARTESIAN_POINT ( 'NONE',  ( 1.432654583217643163, -3.458734124999999437, 17.75000000136560629 ) ) ;
#15854 = DIRECTION ( 'NONE',  ( -1.000000000000000000, -0.000000000000000000, -0.000000000000000000 ) ) ;
#15855 = ORIENTED_EDGE ( 'NONE', *, *, #22949, .F. ) ;
#15856 = CARTESIAN_POINT ( 'NONE',  ( -71.50000000109248788, 7.933012699999995476, 14.14382582708705094 ) ) ;
#15857 = ORIENTED_EDGE ( 'NONE', *, *, #2201, .T. ) ;
#15858 = CARTESIAN_POINT ( 'NONE',  ( 53.59143183416158962, 11.31069182806491291, 12.02818770551463778 ) ) ;
#15859 = CARTESIAN_POINT ( 'NONE',  ( -71.50000000109248788, 7.933012699999995476, 14.14382582708705094 ) ) ;
#15860 = EDGE_CURVE ( 'NONE', #3084, #11384, #14530, .T. ) ;
#15861 = EDGE_CURVE ( 'NONE', #17500, #5746, #18069, .T. ) ;
#15862 = CARTESIAN_POINT ( 'NONE',  ( 19.99999999999999289, 4.500000000000003553, -20.00000000000000355 ) ) ;
#15863 = ORIENTED_EDGE ( 'NONE', *, *, #1037, .F. ) ;
#15864 = DIRECTION ( 'NONE',  ( -1.000000000000000000, 1.224646799147353207E-16, 0.000000000000000000 ) ) ;
#15865 = EDGE_CURVE ( 'NONE', #14872, #633, #16512, .T. ) ;
#15866 = VERTEX_POINT ( 'NONE', #21991 ) ;
#15867 = DIRECTION ( 'NONE',  ( -1.000000000000000000, 0.000000000000000000, 0.000000000000000000 ) ) ;
#15868 = ORIENTED_EDGE ( 'NONE', *, *, #10108, .T. ) ;
#15869 = CARTESIAN_POINT ( 'NONE',  ( 50.75231816583844591, 7.219692298483957771, 17.87654654797633924 ) ) ;
#15870 = CARTESIAN_POINT ( 'NONE',  ( -66.20000000218495018, 9.999999999999998224, 17.49999999999999645 ) ) ;
#15871 = FACE_OUTER_BOUND ( 'NONE', #4625, .T. ) ;
#15872 = DIRECTION ( 'NONE',  ( 0.000000000000000000, 0.000000000000000000, 1.000000000000000000 ) ) ;
#15873 = CARTESIAN_POINT ( 'NONE',  ( -1.432654583217639166, 3.458734125000000770, 15.50000000136560807 ) ) ;
#15874 = CARTESIAN_POINT ( 'NONE',  ( 1.656854249492381470, 4.000000000000000000, 10.81250000273119660 ) ) ;
#15875 = CARTESIAN_POINT ( 'NONE',  ( 58.50000000000000000, 12.12132034355963484, 12.87867965644034740 ) ) ;
#15876 = DIRECTION ( 'NONE',  ( -0.000000000000000000, 1.000000000000000000, -0.000000000000000000 ) ) ;
#15877 = CARTESIAN_POINT ( 'NONE',  ( 51.22106816583844591, 13.02818770551464489, 16.17458954617363531 ) ) ;
#15878 = CARTESIAN_POINT ( 'NONE',  ( -3.458734125000000770, 1.432654583217640498, 1.925000001365597457 ) ) ;
#15879 = CARTESIAN_POINT ( 'NONE',  ( 1.872352939448454495E-15, -3.458734125000000770, 11.93750000136560629 ) ) ;
#15880 = SURFACE_STYLE_USAGE ( .BOTH. , #21347 ) ;
#15881 = ORIENTED_EDGE ( 'NONE', *, *, #10595, .T. ) ;
#15882 = CYLINDRICAL_SURFACE ( 'NONE', #23198, 9.000000000000021316 ) ;
#15883 = PLANE ( 'NONE',  #7453 ) ;
#15884 = ORIENTED_EDGE ( 'NONE', *, *, #5585, .F. ) ;
#15885 = CARTESIAN_POINT ( 'NONE',  ( 58.40625000000000711, 12.99999999999999645, 13.75735931288070191 ) ) ;
#15886 = CARTESIAN_POINT ( 'NONE',  ( 1.656854249492383024, -3.999999999999999112, -0.2624999972688122352 ) ) ;
#15887 = AXIS2_PLACEMENT_3D ( 'NONE', #22914, #3572, #23456 ) ;
#15888 = ADVANCED_FACE ( 'NONE', ( #12932 ), #22105, .T. ) ;
#15889 = ORIENTED_EDGE ( 'NONE', *, *, #17288, .F. ) ;
#15890 = ORIENTED_EDGE ( 'NONE', *, *, #4830, .F. ) ;
#15891 = DIRECTION ( 'NONE',  ( -0.000000000000000000, 0.000000000000000000, 1.000000000000000000 ) ) ;
#15892 = CARTESIAN_POINT ( 'NONE',  ( 38.42689195323381313, -9.000000000000003553, 5.000000000000079936 ) ) ;
#15893 = VERTEX_POINT ( 'NONE', #2358 ) ;
#15894 = CARTESIAN_POINT ( 'NONE',  ( 2.742827927723449299, 3.035229711104609596, -3.433252694550591233 ) ) ;
#15895 = CARTESIAN_POINT ( 'NONE',  ( 4.000000000000001776, -1.656854249492379694, 12.43750000000001066 ) ) ;
#15896 = CARTESIAN_POINT ( 'NONE',  ( 66.50000000109247367, 9.143825827087049163, 17.06698729999999742 ) ) ;
#15897 = AXIS2_PLACEMENT_3D ( 'NONE', #689, #8022, #14994 ) ;
#15898 = CARTESIAN_POINT ( 'NONE',  ( 66.45000000109246230, 12.06698730000000097, 14.99999999999999645 ) ) ;
#15899 = VECTOR ( 'NONE', #5845, 1000.000000000000000 ) ;
#15900 = DIRECTION ( 'NONE',  ( 0.000000000000000000, 0.000000000000000000, 1.000000000000000000 ) ) ;
#15901 = DIRECTION ( 'NONE',  ( 0.000000000000000000, 0.000000000000000000, 1.000000000000000000 ) ) ;
#15902 = CARTESIAN_POINT ( 'NONE',  ( 56.28356816583844591, 8.275094609561968184, 11.02818770551464667 ) ) ;
#15903 = CARTESIAN_POINT ( 'NONE',  ( -1.432654583217640276, 3.458734125000000326, 4.550000001365596347 ) ) ;
#15904 = CARTESIAN_POINT ( 'NONE',  ( 1.025207404391860050E-15, 3.458734125000000326, 13.18750000136560452 ) ) ;
#15905 = DIRECTION ( 'NONE',  ( -1.000000000000000000, -0.000000000000000000, -0.000000000000000000 ) ) ;
#15906 = LINE ( 'NONE', #1626, #5193 ) ;
#15907 = EDGE_LOOP ( 'NONE', ( #11272, #21142, #11281, #3552 ) ) ;
#15908 = CARTESIAN_POINT ( 'NONE',  ( -3.202817526797028247, 1.848609732162391772, 2.039999999999998259 ) ) ;
#15909 = FACE_BOUND ( 'NONE', #9855, .T. ) ;
#15910 = LINE ( 'NONE', #15802, #5063 ) ;
#15911 = EDGE_LOOP ( 'NONE', ( #1211, #21357, #7499, #1685 ) ) ;
#15912 = DIRECTION ( 'NONE',  ( -1.000000000000000000, 0.000000000000000000, 0.000000000000000000 ) ) ;
#15913 = AXIS2_PLACEMENT_3D ( 'NONE', #22834, #17469, #2830 ) ;
#15914 = CARTESIAN_POINT ( 'NONE',  ( 1.799999999999996048, 0.000000000000000000, 0.000000000000000000 ) ) ;
#15915 = ORIENTED_EDGE ( 'NONE', *, *, #16382, .T. ) ;
#15916 = DIRECTION ( 'NONE',  ( 1.000000000000000000, 0.000000000000000000, 0.000000000000000000 ) ) ;
#15917 = ORIENTED_EDGE ( 'NONE', *, *, #6735, .T. ) ;
#15918 = CARTESIAN_POINT ( 'NONE',  ( 58.15856816583844591, 6.028187705514649330, 16.72490539043803182 ) ) ;
#15919 = CARTESIAN_POINT ( 'NONE',  ( 67.55000000218494449, 12.50000000000000000, 13.96446609406725869 ) ) ;
#15920 = VECTOR ( 'NONE', #15722, 1000.000000000000000 ) ;
#15921 = EDGE_CURVE ( 'NONE', #2701, #5919, #20789, .T. ) ;
#15922 = CARTESIAN_POINT ( 'NONE',  ( 2.828427124746192067, -2.828427124746189847, 16.37500000000001066 ) ) ;
#15923 = CARTESIAN_POINT ( 'NONE',  ( -2.345747346278108214, 3.264484291692489215, -0.01223254789873409049 ) ) ;
#15924 = CARTESIAN_POINT ( 'NONE',  ( 68.80000000109247082, 12.06698729999999919, 14.14382582708705094 ) ) ;
#15925 = ORIENTED_EDGE ( 'NONE', *, *, #14945, .T. ) ;
#15926 = PLANE ( 'NONE',  #8401 ) ;
#15927 = DIRECTION ( 'NONE',  ( 1.060575238724910366E-16, -0.4999999999999951705, 0.8660254037844414832 ) ) ;
#15928 = ADVANCED_FACE ( 'NONE', ( #11506 ), #16987, .F. ) ;
#15929 = CARTESIAN_POINT ( 'NONE',  ( 68.05000000109247082, 12.06698730000000097, 14.99999999999999645 ) ) ;
#15930 = CARTESIAN_POINT ( 'NONE',  ( -3.458734124999998993, 1.432654583217640276, 11.37500000136560452 ) ) ;
#15931 = FACE_OUTER_BOUND ( 'NONE', #17851, .T. ) ;
#15932 = CARTESIAN_POINT ( 'NONE',  ( -6.500000000000000888, -2.517290933526015628, -3.443420074781601947 ) ) ;
#15933 = ORIENTED_EDGE ( 'NONE', *, *, #11352, .F. ) ;
#15934 = CARTESIAN_POINT ( 'NONE',  ( -1.656854249492381248, -3.999999999999999112, -1.512499999999997735 ) ) ;
#15935 = CARTESIAN_POINT ( 'NONE',  ( 57.65625000000001421, 7.000000000000002665, 16.24264068711929099 ) ) ;
#15936 = EDGE_LOOP ( 'NONE', ( #15840, #11599 ) ) ;
#15937 = CARTESIAN_POINT ( 'NONE',  ( 4.350525068611871049, -4.993776679985862721, -0.05533025579362501473 ) ) ;
#15938 = CARTESIAN_POINT ( 'NONE',  ( -2.445694354108819635, -2.445694354108820523, -0.1374999986344035974 ) ) ;
#15939 = CARTESIAN_POINT ( 'NONE',  ( -66.05000000109247082, 7.933012699999995476, 14.99999999999999645 ) ) ;
#15940 = ORIENTED_EDGE ( 'NONE', *, *, #20757, .T. ) ;
#15941 = DIRECTION ( 'NONE',  ( 0.000000000000000000, 0.000000000000000000, 1.000000000000000000 ) ) ;
#15942 = ORIENTED_EDGE ( 'NONE', *, *, #18920, .F. ) ;
#15943 = DIRECTION ( 'NONE',  ( -0.000000000000000000, -0.000000000000000000, -1.000000000000000000 ) ) ;
#15944 = VERTEX_POINT ( 'NONE', #2113 ) ;
#15945 = CARTESIAN_POINT ( 'NONE',  ( 1.432654583217641386, 3.458734125000000770, 13.37500000136560452 ) ) ;
#15946 = LINE ( 'NONE', #3122, #5005 ) ;
#15947 = EDGE_CURVE ( 'NONE', #20420, #16436, #11252, .T. ) ;
#15948 = CARTESIAN_POINT ( 'NONE',  ( -65.90000000109246514, 7.933012699999995476, 14.14382582708705094 ) ) ;
#15949 = EDGE_CURVE ( 'NONE', #8014, #11236, #15329, .T. ) ;
#15950 = CARTESIAN_POINT ( 'NONE',  ( 65.70000000109247651, 9.143825827087049163, 17.06698730000000097 ) ) ;
#15951 = CARTESIAN_POINT ( 'NONE',  ( -4.211140560182196957, -2.431303136016552013, -3.745885042887436178 ) ) ;
#15952 = CARTESIAN_POINT ( 'NONE',  ( -68.70000000000000284, 7.499999999999996447, 14.99999999999999645 ) ) ;
#15953 = CARTESIAN_POINT ( 'NONE',  ( -4.000000000000000000, 0.000000000000000000, 0.000000000000000000 ) ) ;
#15954 = EDGE_CURVE ( 'NONE', #19596, #11740, #9690, .T. ) ;
#15955 = CARTESIAN_POINT ( 'NONE',  ( 60.00000000000000000, 11.41727695452472169, 17.97316538709347356 ) ) ;
#15956 = EDGE_CURVE ( 'NONE', #13122, #9843, #13754, .T. ) ;
#15957 = CIRCLE ( 'NONE', #15202, 4.000000000000000000 ) ;
#15958 = CARTESIAN_POINT ( 'NONE',  ( 3.458734125000000770, 4.235727675282972223E-16, -1.512499998634402987 ) ) ;
#15959 = DIRECTION ( 'NONE',  ( 0.000000000000000000, 0.5877852522924742473, -0.8090169943749466741 ) ) ;
#15960 = LINE ( 'NONE', #19648, #3836 ) ;
#15961 = CARTESIAN_POINT ( 'NONE',  ( -2.445694354108819191, 2.445694354108820523, 17.31250000136560274 ) ) ;
#15962 = CARTESIAN_POINT ( 'NONE',  ( -2.000000000000001776, 0.000000000000000000, -6.543750000000021494 ) ) ;
#15963 = ORIENTED_EDGE ( 'NONE', *, *, #12347, .T. ) ;
#15964 = CARTESIAN_POINT ( 'NONE',  ( 4.000000000000000888, 1.656854249492381248, 16.68750000273119838 ) ) ;
#15965 = ORIENTED_EDGE ( 'NONE', *, *, #1966, .F. ) ;
#15966 = CARTESIAN_POINT ( 'NONE',  ( 52.93518183416157541, 9.931948859054372747, 17.99999999999999645 ) ) ;
#15967 = CARTESIAN_POINT ( 'NONE',  ( -67.65000000109247935, 9.999999999999998224, 12.93301269999999192 ) ) ;
#15968 = DIRECTION ( 'NONE',  ( -1.000000000000000000, -1.232595164407830672E-32, 2.052683297350805345E-48 ) ) ;
#15969 = CARTESIAN_POINT ( 'NONE',  ( -27.50000000000000711, 4.500000000000003553, -31.01025403784446510 ) ) ;
#15970 = ORIENTED_EDGE ( 'NONE', *, *, #13349, .T. ) ;
#15971 = AXIS2_PLACEMENT_3D ( 'NONE', #16375, #5943, #5466 ) ;
#15972 = AXIS2_PLACEMENT_3D ( 'NONE', #14666, #7113, #18229 ) ;
#15973 = LINE ( 'NONE', #10370, #9132 ) ;
#15974 = VERTEX_POINT ( 'NONE', #11615 ) ;
#15975 = FACE_OUTER_BOUND ( 'NONE', #15609, .T. ) ;
#15976 = EDGE_LOOP ( 'NONE', ( #1827, #19117, #22960, #13645 ) ) ;
#15977 = CARTESIAN_POINT ( 'NONE',  ( 50.37731816583844591, 7.123453452023657206, 12.21969229848395599 ) ) ;
#15978 = CARTESIAN_POINT ( 'NONE',  ( -67.85000000218495586, 8.964466094067258695, 17.50000000000000355 ) ) ;
#15979 = EDGE_CURVE ( 'NONE', #18055, #7612, #4395, .T. ) ;
#15980 = CARTESIAN_POINT ( 'NONE',  ( -19.99999999999999645, -9.000000000000003553, 5.000000000000079936 ) ) ;
#15981 = AXIS2_PLACEMENT_3D ( 'NONE', #2385, #15230, #17011 ) ;
#15982 = CARTESIAN_POINT ( 'NONE',  ( -1.600000000000004086, 0.000000000000000000, 0.000000000000000000 ) ) ;
#15983 = CARTESIAN_POINT ( 'NONE',  ( 2.445694354108821411, 2.445694354108820523, 15.31250000136560452 ) ) ;
#15984 = CARTESIAN_POINT ( 'NONE',  ( -3.999999999999998224, -1.656854249492383246, 10.18750000273119660 ) ) ;
#15985 = EDGE_CURVE ( 'NONE', #8981, #9536, #15300, .T. ) ;
#15986 = CARTESIAN_POINT ( 'NONE',  ( 57.18750000000000000, 9.999999999999989342, 11.99999999999999467 ) ) ;
#15987 = AXIS2_PLACEMENT_3D ( 'NONE', #22453, #2223, #74 ) ;
#15988 = LINE ( 'NONE', #23274, #4888 ) ;
#15989 = VECTOR ( 'NONE', #7902, 1000.000000000000000 ) ;
#15990 = EDGE_CURVE ( 'NONE', #10158, #2314, #12190, .T. ) ;
#15991 = CARTESIAN_POINT ( 'NONE',  ( 56.71875000000000711, 13.00000000000000711, 16.24264068711927322 ) ) ;
#15992 = CARTESIAN_POINT ( 'NONE',  ( 3.458734125000000770, 1.432654583217640498, 1.550000001365597013 ) ) ;
#15993 = CARTESIAN_POINT ( 'NONE',  ( 0.000000000000000000, 0.000000000000000000, 0.000000000000000000 ) ) ;
#15994 = CARTESIAN_POINT ( 'NONE',  ( 70.30000000218494449, 8.232233047033627571, 16.76776695296636532 ) ) ;
#15995 = EDGE_LOOP ( 'NONE', ( #16100, #11722, #10872, #20507 ) ) ;
#15996 = LINE ( 'NONE', #21233, #18996 ) ;
#15997 = CARTESIAN_POINT ( 'NONE',  ( -65.00000000000000000, -10.00000000000000178, 12.49999999999999467 ) ) ;
#15998 = EDGE_LOOP ( 'NONE', ( #12522, #6658, #8799, #9654 ) ) ;
#15999 = CARTESIAN_POINT ( 'NONE',  ( 59.90625000000000711, 12.99999999999999645, 13.75735931288070191 ) ) ;
#16000 =( NAMED_UNIT ( * ) SI_UNIT ( $, .STERADIAN. ) SOLID_ANGLE_UNIT ( ) );
#16001 = CARTESIAN_POINT ( 'NONE',  ( -2.828427124746190291, 2.828427124746190291, 1.300000002731187543 ) ) ;
#16002 = LINE ( 'NONE', #19927, #11704 ) ;
#16003 = VERTEX_POINT ( 'NONE', #7656 ) ;
#16004 = ORIENTED_EDGE ( 'NONE', *, *, #5404, .T. ) ;
#16005 = AXIS2_PLACEMENT_3D ( 'NONE', #18235, #145, #14793 ) ;
#16006 = DIRECTION ( 'NONE',  ( -1.000000000000000000, 0.000000000000000000, -0.000000000000000000 ) ) ;
#16007 = ORIENTED_EDGE ( 'NONE', *, *, #2436, .T. ) ;
#16008 = DIRECTION ( 'NONE',  ( -1.000000000000000000, -7.703719777548943412E-32, 0.000000000000000000 ) ) ;
#16009 = VECTOR ( 'NONE', #12426, 1000.000000000000000 ) ;
#16010 = COLOUR_RGB ( '', 0.31764706, 0.68627451, 0.89019608) ;
#16011 = CARTESIAN_POINT ( 'NONE',  ( 2.828427124746192067, -2.828427124746189847, 11.37500000000001066 ) ) ;
#16012 = ORIENTED_EDGE ( 'NONE', *, *, #21597, .T. ) ;
#16013 = CARTESIAN_POINT ( 'NONE',  ( 66.60000000109248219, 7.933012699999995476, 15.85617417291294196 ) ) ;
#16014 = CARTESIAN_POINT ( 'NONE',  ( 66.40000000109247935, 12.06698730000000275, 14.14382582708705094 ) ) ;
#16015 = EDGE_CURVE ( 'NONE', #990, #462, #11734, .T. ) ;
#16016 = EDGE_CURVE ( 'NONE', #14633, #11306, #20313, .T. ) ;
#16017 = VECTOR ( 'NONE', #348, 1000.000000000000000 ) ;
#16018 = CARTESIAN_POINT ( 'NONE',  ( 69.59999999999999432, 8.232233047033629347, 13.23223304703362402 ) ) ;
#16019 = CARTESIAN_POINT ( 'NONE',  ( 52.50000000000000711, 12.82842712474617741, 12.17157287525379239 ) ) ;
#16020 = CARTESIAN_POINT ( 'NONE',  ( 6.353591512924457348E-16, -3.458734125000000326, 4.987500001365595459 ) ) ;
#16021 = DIRECTION ( 'NONE',  ( -1.000000000000000000, 0.000000000000000000, 0.000000000000000000 ) ) ;
#16022 = CARTESIAN_POINT ( 'NONE',  ( 1.025207404391860050E-15, 3.458734125000000326, 14.18750000136560452 ) ) ;
#16023 = FACE_OUTER_BOUND ( 'NONE', #11857, .T. ) ;
#16024 = VECTOR ( 'NONE', #17707, 1000.000000000000000 ) ;
#16025 = CYLINDRICAL_SURFACE ( 'NONE', #11728, 4.000000000000000000 ) ;
#16026 = ORIENTED_EDGE ( 'NONE', *, *, #22195, .F. ) ;
#16027 = CARTESIAN_POINT ( 'NONE',  ( -2.031236510114588611, 3.247785564556652460, 2.039999999999996927 ) ) ;
#16028 = AXIS2_PLACEMENT_3D ( 'NONE', #16385, #16731, #11004 ) ;
#16029 = DIRECTION ( 'NONE',  ( -1.000000000000000000, 0.000000000000000000, 0.000000000000000000 ) ) ;
#16030 = PLANE ( 'NONE',  #7470 ) ;
#16031 = ORIENTED_EDGE ( 'NONE', *, *, #3043, .T. ) ;
#16032 = FACE_OUTER_BOUND ( 'NONE', #15321, .T. ) ;
#16033 = CARTESIAN_POINT ( 'NONE',  ( 16.43574340323381122, -9.000000000000001776, 10.00000000000008882 ) ) ;
#16034 = VECTOR ( 'NONE', #23236, 1000.000000000000000 ) ;
#16035 = FACE_OUTER_BOUND ( 'NONE', #15907, .T. ) ;
#16036 = VERTEX_POINT ( 'NONE', #448 ) ;
#16037 = CARTESIAN_POINT ( 'NONE',  ( -68.30000000218494449, 11.76776695296636888, 13.23223304703362579 ) ) ;
#16038 = EDGE_LOOP ( 'NONE', ( #19309, #13636, #15571, #16863 ) ) ;
#16039 = AXIS2_PLACEMENT_3D ( 'NONE', #21574, #4957, #8681 ) ;
#16040 = CARTESIAN_POINT ( 'NONE',  ( 54.18750000000000711, 9.999999999999978684, 10.99999999999999645 ) ) ;
#16041 = CARTESIAN_POINT ( 'NONE',  ( 68.90000000218495302, 8.232233047033629347, 13.23223304703362402 ) ) ;
#16042 = DIRECTION ( 'NONE',  ( -1.000000000000000000, -0.000000000000000000, -0.000000000000000000 ) ) ;
#16043 = FACE_OUTER_BOUND ( 'NONE', #5411, .T. ) ;
#16044 = DIRECTION ( 'NONE',  ( 0.3420201433256622736, 0.9396926207859106484, 0.000000000000000000 ) ) ;
#16045 = ORIENTED_EDGE ( 'NONE', *, *, #3169, .F. ) ;
#16046 = AXIS2_PLACEMENT_3D ( 'NONE', #22844, #13778, #8379 ) ;
#16047 = FACE_OUTER_BOUND ( 'NONE', #13842, .T. ) ;
#16048 = LINE ( 'NONE', #6947, #5689 ) ;
#16049 = AXIS2_PLACEMENT_3D ( 'NONE', #13899, #2735, #6812 ) ;
#16050 = DIRECTION ( 'NONE',  ( -1.000000000000000000, 0.000000000000000000, 1.224646799147353207E-16 ) ) ;
#16051 = CARTESIAN_POINT ( 'NONE',  ( 1.432654583217641386, 3.458734125000000770, 19.37500000136560274 ) ) ;
#16052 = DIRECTION ( 'NONE',  ( 1.000000000000000000, 4.625929269271486900E-16, -1.224646799147353207E-16 ) ) ;
#16053 = CIRCLE ( 'NONE', #14926, 8.749000000000002331 ) ;
#16054 = FACE_OUTER_BOUND ( 'NONE', #14192, .T. ) ;
#16055 = ORIENTED_EDGE ( 'NONE', *, *, #877, .T. ) ;
#16056 = CARTESIAN_POINT ( 'NONE',  ( -20.00005079999999680, 0.000000000000000000, 0.000000000000000000 ) ) ;
#16057 = CARTESIAN_POINT ( 'NONE',  ( 59.81250000000000711, 13.00000000000000000, 14.99999999999998757 ) ) ;
#16058 = SURFACE_STYLE_USAGE ( .BOTH. , #19624 ) ;
#16059 = ORIENTED_EDGE ( 'NONE', *, *, #11893, .F. ) ;
#16060 = EDGE_CURVE ( 'NONE', #18029, #10634, #4948, .T. ) ;
#16061 = CARTESIAN_POINT ( 'NONE',  ( 15.83013239071656741, -8.974600000000002353, 5.000000000000079936 ) ) ;
#16062 = CARTESIAN_POINT ( 'NONE',  ( -3.458734125000000326, 0.000000000000000000, -1.262499998634402765 ) ) ;
#16063 = CARTESIAN_POINT ( 'NONE',  ( 4.999999999999999112, 1.464956435139541879, 10.90201369670499076 ) ) ;
#16064 = VECTOR ( 'NONE', #7128, 1000.000000000000000 ) ;
#16065 = VERTEX_POINT ( 'NONE', #2586 ) ;
#16066 = CARTESIAN_POINT ( 'NONE',  ( -10.00000000000000000, 0.000000000000000000, 0.000000000000000000 ) ) ;
#16067 = VERTEX_POINT ( 'NONE', #7774 ) ;
#16068 = CARTESIAN_POINT ( 'NONE',  ( 0.000000000000000000, 9.241976615262160522, 2.300561732649595736 ) ) ;
#16069 = EDGE_LOOP ( 'NONE', ( #16130, #1810, #7821, #13912 ) ) ;
#16070 = CARTESIAN_POINT ( 'NONE',  ( 4.000000000000000888, 1.656854249492381248, 17.56250000000001421 ) ) ;
#16071 = AXIS2_PLACEMENT_3D ( 'NONE', #21986, #1526, #16161 ) ;
#16072 = DIRECTION ( 'NONE',  ( -1.000000000000000000, 0.000000000000000000, 0.000000000000000000 ) ) ;
#16073 = AXIS2_PLACEMENT_3D ( 'NONE', #3071, #1256, #17580 ) ;
#16074 = CARTESIAN_POINT ( 'NONE',  ( 4.999999999999999112, 9.314797388894893615, 1.239665997526919083 ) ) ;
#16075 = SURFACE_STYLE_FILL_AREA ( #5630 ) ;
#16076 = DIRECTION ( 'NONE',  ( -1.000000000000000000, -0.000000000000000000, 0.000000000000000000 ) ) ;
#16077 = AXIS2_PLACEMENT_3D ( 'NONE', #18273, #1857, #7516 ) ;
#16078 = CARTESIAN_POINT ( 'NONE',  ( -71.14999999999999147, 7.499999999999995559, 13.96446609406725692 ) ) ;
#16079 = CIRCLE ( 'NONE', #12669, 4.000000000000001776 ) ;
#16080 = FACE_OUTER_BOUND ( 'NONE', #1512, .T. ) ;
#16081 = CARTESIAN_POINT ( 'NONE',  ( 60.00000000000001421, 13.54696164955606008, 13.15578628297699382 ) ) ;
#16082 = CARTESIAN_POINT ( 'NONE',  ( 6.353591512924457348E-16, -3.458734125000000770, -1.762499998634403209 ) ) ;
#16083 = CARTESIAN_POINT ( 'NONE',  ( 4.999999999999999112, -3.174628368996021521, -8.152713396088794084 ) ) ;
#16084 = DIRECTION ( 'NONE',  ( 0.000000000000000000, 1.000000000000000000, 3.469446951953611822E-15 ) ) ;
#16085 = CARTESIAN_POINT ( 'NONE',  ( -3.458734124999998993, 0.000000000000000000, 18.43750000136560629 ) ) ;
#16086 = DIRECTION ( 'NONE',  ( 1.000000000000000000, 7.703719777548943412E-32, 0.000000000000000000 ) ) ;
#16087 = EDGE_LOOP ( 'NONE', ( #15373, #15785, #8090, #22824 ) ) ;
#16088 = EDGE_CURVE ( 'NONE', #8446, #19331, #15092, .T. ) ;
#16089 = CARTESIAN_POINT ( 'NONE',  ( -70.95000000109247651, 11.46158073645647235, 13.53841926354352232 ) ) ;
#16090 = ORIENTED_EDGE ( 'NONE', *, *, #17460, .T. ) ;
#16091 = CARTESIAN_POINT ( 'NONE',  ( 59.49768183416157541, 12.87654654797631792, 12.21969229848393113 ) ) ;
#16092 = CARTESIAN_POINT ( 'NONE',  ( -67.90000000109246514, 12.06698730000000275, 15.85617417291294196 ) ) ;
#16093 = CARTESIAN_POINT ( 'NONE',  ( 1.234698900865588551E-17, 0.000000000000000000, -1.999999999999991340 ) ) ;
#16094 = EDGE_CURVE ( 'NONE', #15866, #3630, #21369, .T. ) ;
#16095 = CARTESIAN_POINT ( 'NONE',  ( -1.432654583217640942, -3.458734124999999882, -2.074999998634404097 ) ) ;
#16096 = ORIENTED_EDGE ( 'NONE', *, *, #21498, .T. ) ;
#16097 = CIRCLE ( 'NONE', #6534, 11.00000000000000000 ) ;
#16098 = CARTESIAN_POINT ( 'NONE',  ( -10.13078668033273999, -11.25000000000000355, 5.000000000000079936 ) ) ;
#16099 = VECTOR ( 'NONE', #15602, 1000.000000000000000 ) ;
#16100 = ORIENTED_EDGE ( 'NONE', *, *, #9858, .F. ) ;
#16101 = LINE ( 'NONE', #14308, #647 ) ;
#16102 = VERTEX_POINT ( 'NONE', #5963 ) ;
#16103 = ADVANCED_FACE ( 'NONE', ( #4281, #19236, #8595 ), #4994, .F. ) ;
#16104 = CARTESIAN_POINT ( 'NONE',  ( 50.56481816583844591, 6.999999999999998224, 15.06805114094563436 ) ) ;
#16105 = CARTESIAN_POINT ( 'NONE',  ( -66.90000000218495302, 11.76776695296636888, 16.76776695296636532 ) ) ;
#16106 = CARTESIAN_POINT ( 'NONE',  ( -3.416564614606786066, 1.811858101813906607, -3.557290855993161305 ) ) ;
#16107 = CARTESIAN_POINT ( 'NONE',  ( 4.714285714285714413, 0.000000000000000000, 3.059999999999998277 ) ) ;
#16108 = CARTESIAN_POINT ( 'NONE',  ( 2.445694354108821411, 2.445694354108820523, 16.31250000136560629 ) ) ;
#16109 = CARTESIAN_POINT ( 'NONE',  ( -3.999999999999999112, 0.000000000000000000, 11.12500000273119660 ) ) ;
#16110 = CARTESIAN_POINT ( 'NONE',  ( 58.96875000000000711, 6.999999999999992895, 13.75735931288071967 ) ) ;
#16111 = AXIS2_PLACEMENT_3D ( 'NONE', #5255, #10681, #10565 ) ;
#16112 = DIRECTION ( 'NONE',  ( -0.000000000000000000, -0.000000000000000000, 1.000000000000000000 ) ) ;
#16113 = CARTESIAN_POINT ( 'NONE',  ( 59.53125000000000000, 11.24264068711929276, 18.00000000000000355 ) ) ;
#16114 = CARTESIAN_POINT ( 'NONE',  ( 3.458734125000000770, 1.432654583217640498, 3.550000001365598568 ) ) ;
#16115 = CARTESIAN_POINT ( 'NONE',  ( -3.270501301980698550, -1.125461230421587633, 2.040000000000001812 ) ) ;
#16116 = DIRECTION ( 'NONE',  ( 0.000000000000000000, 0.000000000000000000, -1.000000000000000000 ) ) ;
#16117 = ORIENTED_EDGE ( 'NONE', *, *, #5302, .F. ) ;
#16118 = DIRECTION ( 'NONE',  ( -0.000000000000000000, 1.000000000000000000, -0.000000000000000000 ) ) ;
#16119 = CARTESIAN_POINT ( 'NONE',  ( 0.000000000000000000, 0.000000000000000000, -25.03750572909317285 ) ) ;
#16120 = ORIENTED_EDGE ( 'NONE', *, *, #17080, .F. ) ;
#16121 = PLANE ( 'NONE',  #2313 ) ;
#16122 =( NAMED_UNIT ( * ) SI_UNIT ( $, .STERADIAN. ) SOLID_ANGLE_UNIT ( ) );
#16123 = CARTESIAN_POINT ( 'NONE',  ( -4.000000000000000000, -1.656854249492383246, -0.5124999972688124572 ) ) ;
#16124 = ADVANCED_FACE ( 'NONE', ( #22710 ), #19472, .T. ) ;
#16125 = DIRECTION ( 'NONE',  ( 0.000000000000000000, 0.000000000000000000, 1.000000000000000000 ) ) ;
#16126 = ORIENTED_EDGE ( 'NONE', *, *, #12030, .T. ) ;
#16127 = CARTESIAN_POINT ( 'NONE',  ( -3.999999999999999112, 1.656854249492380804, 18.93750000000000711 ) ) ;
#16128 = ORIENTED_EDGE ( 'NONE', *, *, #247, .F. ) ;
#16129 = CARTESIAN_POINT ( 'NONE',  ( -72.25000000109247367, 9.999999999999998224, 17.06698730000000097 ) ) ;
#16130 = ORIENTED_EDGE ( 'NONE', *, *, #4470, .F. ) ;
#16131 = ADVANCED_FACE ( 'NONE', ( #8488 ), #15792, .T. ) ;
#16132 = CARTESIAN_POINT ( 'NONE',  ( -19.99999999999999645, -9.000000000000003553, 5.000000000000079936 ) ) ;
#16133 = VECTOR ( 'NONE', #14505, 1000.000000000000000 ) ;
#16134 = EDGE_CURVE ( 'NONE', #14520, #17845, #20900, .T. ) ;
#16135 = CARTESIAN_POINT ( 'NONE',  ( 9.920644283265380691E-16, 4.000000000000000000, 11.75000000000001066 ) ) ;
#16136 = ORIENTED_EDGE ( 'NONE', *, *, #17133, .F. ) ;
#16137 = CARTESIAN_POINT ( 'NONE',  ( 66.05000000109247082, 9.999999999999998224, 12.93301269999999192 ) ) ;
#16138 = CARTESIAN_POINT ( 'NONE',  ( 70.89999999999999147, 9.999999999999998224, 17.49999999999999645 ) ) ;
#16139 = FACE_OUTER_BOUND ( 'NONE', #20141, .T. ) ;
#16140 = CARTESIAN_POINT ( 'NONE',  ( 36.10423233033275636, -11.25000000000000355, 5.000000000000079936 ) ) ;
#16141 = CARTESIAN_POINT ( 'NONE',  ( 58.15856816583844591, 6.028187705514649330, 16.72490539043803182 ) ) ;
#16142 = CARTESIAN_POINT ( 'NONE',  ( -3.458734125000000326, 1.432654583217640276, 4.675000001365594571 ) ) ;
#16143 = CARTESIAN_POINT ( 'NONE',  ( 3.458734125000001214, 4.235727675282971730E-16, 13.93750000136560629 ) ) ;
#16144 = DIRECTION ( 'NONE',  ( 0.000000000000000000, 0.000000000000000000, 1.000000000000000000 ) ) ;
#16145 = CARTESIAN_POINT ( 'NONE',  ( -70.55000000218494449, 8.964466094067205404, 12.50000000000004263 ) ) ;
#16146 = ORIENTED_EDGE ( 'NONE', *, *, #9792, .F. ) ;
#16147 = CYLINDRICAL_SURFACE ( 'NONE', #11107, 4.000000000000001776 ) ;
#16148 = PLANE ( 'NONE',  #7883 ) ;
#16149 = CARTESIAN_POINT ( 'NONE',  ( 4.000000000000000888, -1.656854249492379694, -1.262499999999997513 ) ) ;
#16150 = EDGE_LOOP ( 'NONE', ( #11630, #19933, #3896, #2539 ) ) ;
#16151 = DIRECTION ( 'NONE',  ( 0.000000000000000000, 0.8090169943749485615, -0.5877852522924714718 ) ) ;
#16152 = EDGE_CURVE ( 'NONE', #23005, #22090, #6789, .T. ) ;
#16153 = ADVANCED_FACE ( 'NONE', ( #801 ), #19586, .T. ) ;
#16154 = CARTESIAN_POINT ( 'NONE',  ( 71.00000000218494733, 9.999999999999998224, 17.49999999999999645 ) ) ;
#16155 = ORIENTED_EDGE ( 'NONE', *, *, #11023, .F. ) ;
#16156 = CARTESIAN_POINT ( 'NONE',  ( 66.00000000218494733, 12.50000000000000000, 14.99999999999999645 ) ) ;
#16157 = VERTEX_POINT ( 'NONE', #19126 ) ;
#16158 = EDGE_CURVE ( 'NONE', #14838, #1746, #1517, .T. ) ;
#16159 = CARTESIAN_POINT ( 'NONE',  ( 52.50000000000000711, 12.82842712474617741, 12.17157287525379239 ) ) ;
#16160 = CARTESIAN_POINT ( 'NONE',  ( 67.90000000218495302, 8.232233047033627571, 16.76776695296636532 ) ) ;
#16161 = DIRECTION ( 'NONE',  ( 0.000000000000000000, 0.000000000000000000, 1.000000000000000000 ) ) ;
#16162 =( BOUNDED_CURVE ( )  B_SPLINE_CURVE ( 2, ( #13505, #22933, #2921, #23048, #9785, #21118, #10271, #15427, #4262 ),
 .UNSPECIFIED., .F., .F. ) 
 B_SPLINE_CURVE_WITH_KNOTS ( ( 3, 2, 2, 2, 3 ),
 ( 0.8000000000000000444, 0.8125000000000000000, 0.8249999999999999556, 0.8375000000000000222, 0.8499999999999999778 ),
 .UNSPECIFIED. ) 
 CURVE ( )  GEOMETRIC_REPRESENTATION_ITEM ( )  RATIONAL_B_SPLINE_CURVE ( ( 1.000000000000000000, 0.9238795325112867385, 1.000000000000000000, 0.9238795325112867385, 1.000000000000000000, 0.9238795325112867385, 1.000000000000000000, 0.9238795325112867385, 1.000000000000000000 ) ) 
 REPRESENTATION_ITEM ( '' )  );
#16163 = DIRECTION ( 'NONE',  ( -7.087422195345011518E-32, -1.000000000000000000, -0.000000000000000000 ) ) ;
#16164 = PLANE ( 'NONE',  #11829 ) ;
#16165 = ORIENTED_EDGE ( 'NONE', *, *, #11617, .T. ) ;
#16166 = LINE ( 'NONE', #23576, #17575 ) ;
#16167 = CARTESIAN_POINT ( 'NONE',  ( 58.27893183416158962, 8.411196891453236901, 10.97181229448535511 ) ) ;
#16168 = LINE ( 'NONE', #12596, #19079 ) ;
#16169 = CARTESIAN_POINT ( 'NONE',  ( 66.85000000109246798, 7.933012699999995476, 14.99999999999999645 ) ) ;
#16170 = CARTESIAN_POINT ( 'NONE',  ( -68.99999999999998579, 11.76776695296636888, 13.23223304703362579 ) ) ;
#16171 = CARTESIAN_POINT ( 'NONE',  ( -6.500000000000000000, -0.6341575537611434665, -3.700000000000001066 ) ) ;
#16172 = ORIENTED_EDGE ( 'NONE', *, *, #5258, .F. ) ;
#16173 = DIRECTION ( 'NONE',  ( 0.000000000000000000, 0.000000000000000000, -1.000000000000000000 ) ) ;
#16174 = CARTESIAN_POINT ( 'NONE',  ( 58.12500000000000000, 12.12132034355964727, 17.12132034355963484 ) ) ;
#16175 = CARTESIAN_POINT ( 'NONE',  ( 4.000000000000000888, 4.898587196589412829E-16, 10.62500000273119660 ) ) ;
#16176 = AXIS2_PLACEMENT_3D ( 'NONE', #13179, #16883, #11516 ) ;
#16177 = EDGE_LOOP ( 'NONE', ( #7297, #21846, #14450, #20076 ) ) ;
#16178 = DIRECTION ( 'NONE',  ( -1.000000000000000000, -0.000000000000000000, -0.000000000000000000 ) ) ;
#16179 = CARTESIAN_POINT ( 'NONE',  ( 3.458734125000000326, 1.432654583217640498, -1.699999998634404097 ) ) ;
#16180 = FACE_OUTER_BOUND ( 'NONE', #3310, .T. ) ;
#16181 = ORIENTED_EDGE ( 'NONE', *, *, #15551, .F. ) ;
#16182 = CARTESIAN_POINT ( 'NONE',  ( 0.1129242967662022479, -9.000000000000001776, 5.000000000000079936 ) ) ;
#16183 = ORIENTED_EDGE ( 'NONE', *, *, #7742, .F. ) ;
#16184 = CARTESIAN_POINT ( 'NONE',  ( -1.656854249492379472, 4.000000000000000000, 12.93750000273119660 ) ) ;
#16185 = CARTESIAN_POINT ( 'NONE',  ( 1.656854249492381470, 4.000000000000000000, 19.68750000000001066 ) ) ;
#16186 = DIRECTION ( 'NONE',  ( 0.9396926207859138680, 1.150791560227856926E-16, -0.3420201433256536139 ) ) ;
#16187 = CARTESIAN_POINT ( 'NONE',  ( -1.489200000000000079, 0.000000000000000000, -6.760799999999997034 ) ) ;
#16188 = DIRECTION ( 'NONE',  ( 1.000000000000000000, 0.000000000000000000, 0.000000000000000000 ) ) ;
#16189 = DIRECTION ( 'NONE',  ( 7.087422195345011518E-32, 1.000000000000000000, -0.000000000000000000 ) ) ;
#16190 = ADVANCED_FACE ( 'NONE', ( #2826 ), #17464, .F. ) ;
#16191 = CARTESIAN_POINT ( 'NONE',  ( -68.49999999999998579, 9.999999999999998224, 17.49999999999999645 ) ) ;
#16192 = AXIS2_PLACEMENT_3D ( 'NONE', #10147, #10033, #17321 ) ;
#16193 = CYLINDRICAL_SURFACE ( 'NONE', #8395, 6.499999999999999112 ) ;
#16194 = CARTESIAN_POINT ( 'NONE',  ( 60.00000000000000000, 12.85334760243663155, 16.18560892438961929 ) ) ;
#16195 = CARTESIAN_POINT ( 'NONE',  ( -4.207491450040567571, 2.029819825146470524, -3.671670828759566074 ) ) ;
#16196 =( BOUNDED_CURVE ( )  B_SPLINE_CURVE ( 2, ( #14023, #9974, #22992, #4670, #2631, #1065, #19383, #10331, #21171 ),
 .UNSPECIFIED., .F., .F. ) 
 B_SPLINE_CURVE_WITH_KNOTS ( ( 3, 2, 2, 2, 3 ),
 ( 0.4000000000000000222, 0.4124999999999999778, 0.4249999999999999889, 0.4375000000000000000, 0.4500000000000000111 ),
 .UNSPECIFIED. ) 
 CURVE ( )  GEOMETRIC_REPRESENTATION_ITEM ( )  RATIONAL_B_SPLINE_CURVE ( ( 1.000000000000000000, 0.9238795325112867385, 1.000000000000000000, 0.9238795325112867385, 1.000000000000000000, 0.9238795325112867385, 1.000000000000000000, 0.9238795325112867385, 1.000000000000000000 ) ) 
 REPRESENTATION_ITEM ( '' )  );
#16197 = CARTESIAN_POINT ( 'NONE',  ( 2.828427124746189847, 2.828427124746190291, 5.925000000000001599 ) ) ;
#16198 = CARTESIAN_POINT ( 'NONE',  ( -67.65000000218496723, 12.50000000000000000, 16.03553390593273775 ) ) ;
#16199 = CARTESIAN_POINT ( 'NONE',  ( -0.9413949561959077394, -0.3373062947069099260, -19.99999999999999645 ) ) ;
#16200 = CARTESIAN_POINT ( 'NONE',  ( -3.458734124999998993, 0.000000000000000000, 17.43750000136560274 ) ) ;
#16201 = CARTESIAN_POINT ( 'NONE',  ( 2.500000000000000000, 0.000000000000000000, 2.041999999999999815 ) ) ;
#16202 = ORIENTED_EDGE ( 'NONE', *, *, #7038, .T. ) ;
#16203 = CARTESIAN_POINT ( 'NONE',  ( -71.10000000109246798, 12.06698729999999919, 15.85617417291294196 ) ) ;
#16204 = ORIENTED_EDGE ( 'NONE', *, *, #3794, .T. ) ;
#16205 = CARTESIAN_POINT ( 'NONE',  ( 55.74768183416157541, 7.123453452023678523, 17.78030770151605822 ) ) ;
#16206 = CARTESIAN_POINT ( 'NONE',  ( -67.70000000109246230, 10.85617417291294551, 12.93301269999999370 ) ) ;
#16207 = DIRECTION ( 'NONE',  ( 0.000000000000000000, 0.000000000000000000, 1.000000000000000000 ) ) ;
#16208 = DIRECTION ( 'NONE',  ( 0.000000000000000000, -0.8090169943749403458, -0.5877852522924830181 ) ) ;
#16209 = ORIENTED_EDGE ( 'NONE', *, *, #11352, .T. ) ;
#16210 = AXIS2_PLACEMENT_3D ( 'NONE', #4620, #15776, #19222 ) ;
#16211 = VECTOR ( 'NONE', #2248, 1000.000000000000000 ) ;
#16212 = VERTEX_POINT ( 'NONE', #13637 ) ;
#16213 = DIRECTION ( 'NONE',  ( 0.000000000000000000, 0.000000000000000000, -1.000000000000000000 ) ) ;
#16214 = ORIENTED_EDGE ( 'NONE', *, *, #20930, .T. ) ;
#16215 = CARTESIAN_POINT ( 'NONE',  ( 59.43750000000000711, 10.00000000000000711, 17.99999999999999645 ) ) ;
#16216 = CARTESIAN_POINT ( 'NONE',  ( -70.75000000109247367, 8.538419263543524096, 13.53841926354352054 ) ) ;
#16217 = EDGE_CURVE ( 'NONE', #17794, #19948, #19486, .T. ) ;
#16218 = CARTESIAN_POINT ( 'NONE',  ( -70.05000000109247082, 7.933012699999995476, 14.99999999999999645 ) ) ;
#16219 = CARTESIAN_POINT ( 'NONE',  ( -1.432654583217639832, -3.458734125000000326, 16.87500000136560629 ) ) ;
#16220 = ADVANCED_FACE ( 'NONE', ( #6322 ), #1027, .T. ) ;
#16221 = CARTESIAN_POINT ( 'NONE',  ( 4.000000000000001776, -1.656854249492379694, 10.56250000273119660 ) ) ;
#16222 = CARTESIAN_POINT ( 'NONE',  ( 55.03125000000000000, 11.24264068711929276, 18.00000000000000355 ) ) ;
#16223 = CYLINDRICAL_SURFACE ( 'NONE', #14067, 2.649999999999999467 ) ;
#16224 = CARTESIAN_POINT ( 'NONE',  ( 59.06250000000000711, 6.999999999999997335, 15.00000000000000533 ) ) ;
#16225 = LINE ( 'NONE', #14438, #14202 ) ;
#16226 = CARTESIAN_POINT ( 'NONE',  ( -3.999999999999999112, 0.000000000000000000, 18.12500000273119483 ) ) ;
#16227 = EDGE_CURVE ( 'NONE', #23080, #20778, #13023, .T. ) ;
#16228 = CARTESIAN_POINT ( 'NONE',  ( 0.000000000000000000, 0.000000000000000000, 0.000000000000000000 ) ) ;
#16229 = VERTEX_POINT ( 'NONE', #6441 ) ;
#16230 = CARTESIAN_POINT ( 'NONE',  ( -4.000000000000000000, -1.942223658245633811, -0.3516579909967644246 ) ) ;
#16231 = DIRECTION ( 'NONE',  ( 7.087422195345011518E-32, 1.000000000000000000, -0.000000000000000000 ) ) ;
#16232 = ORIENTED_EDGE ( 'NONE', *, *, #15009, .F. ) ;
#16233 = CARTESIAN_POINT ( 'NONE',  ( 53.25000000000000711, 7.878679656440361612, 17.12132034355964549 ) ) ;
#16234 = CARTESIAN_POINT ( 'NONE',  ( 2.828427124746189847, 2.828427124746190291, 0.05000000273118650196 ) ) ;
#16235 = FACE_OUTER_BOUND ( 'NONE', #17768, .T. ) ;
#16236 = ORIENTED_EDGE ( 'NONE', *, *, #20893, .T. ) ;
#16237 = CARTESIAN_POINT ( 'NONE',  ( -3.999999999999999112, 1.656854249492380804, 16.93750000000001066 ) ) ;
#16238 = EDGE_LOOP ( 'NONE', ( #16357, #17994, #8504, #11833 ) ) ;
#16239 = SURFACE_STYLE_USAGE ( .BOTH. , #21478 ) ;
#16240 = VECTOR ( 'NONE', #19471, 1000.000000000000000 ) ;
#16241 = PLANE ( 'NONE',  #12590 ) ;
#16242 = ORIENTED_EDGE ( 'NONE', *, *, #20190, .T. ) ;
#16243 = CARTESIAN_POINT ( 'NONE',  ( 65.00000000000000000, 15.00000000000000000, 10.00000000000007105 ) ) ;
#16244 = CARTESIAN_POINT ( 'NONE',  ( 4.000000000000000888, 4.898587196589412829E-16, 12.50000000000001066 ) ) ;
#16245 = VERTEX_POINT ( 'NONE', #13760 ) ;
#16246 = DIRECTION ( 'NONE',  ( -0.000000000000000000, -0.000000000000000000, 1.000000000000000000 ) ) ;
#16247 = EDGE_CURVE ( 'NONE', #11624, #16281, #8814, .T. ) ;
#16248 = CARTESIAN_POINT ( 'NONE',  ( 66.05000000109247082, 7.933012699999995476, 14.99999999999999645 ) ) ;
#16249 = EDGE_CURVE ( 'NONE', #4081, #16269, #11882, .T. ) ;
#16250 = DIRECTION ( 'NONE',  ( 0.000000000000000000, 0.000000000000000000, -1.000000000000000000 ) ) ;
#16252 = CARTESIAN_POINT ( 'NONE',  ( 0.000000000000000000, -7.360373001730883935, -4.729683950898952105 ) ) ;
#16251 = AXIS2_PLACEMENT_3D ( 'NONE', #8939, #19452, #21586 ) ;
#16253 = CARTESIAN_POINT ( 'NONE',  ( 58.53356816583845301, 11.72490539043803004, 18.97181229448534268 ) ) ;
#16254 = AXIS2_PLACEMENT_3D ( 'NONE', #1405, #17726, #23342 ) ;
#16255 = CARTESIAN_POINT ( 'NONE',  ( 3.458734125000000326, 4.235727675282971730E-16, 0.2375000013655967357 ) ) ;
#16256 = EDGE_CURVE ( 'NONE', #14554, #16229, #2270, .T. ) ;
#16257 =( NAMED_UNIT ( * ) PLANE_ANGLE_UNIT ( ) SI_UNIT ( $, .RADIAN. ) );
#16258 = CARTESIAN_POINT ( 'NONE',  ( -3.458734124999998105, -1.432654583217642275, 14.50000000136560629 ) ) ;
#16259 = LINE ( 'NONE', #23548, #17803 ) ;
#16260 = ADVANCED_FACE ( 'NONE', ( #6675 ), #13988, .F. ) ;
#16261 = CARTESIAN_POINT ( 'NONE',  ( -70.25000000218493312, 8.964466094067294222, 17.50000000000003908 ) ) ;
#16262 = ORIENTED_EDGE ( 'NONE', *, *, #3968, .T. ) ;
#16263 = DIRECTION ( 'NONE',  ( 0.000000000000000000, 0.000000000000000000, 1.000000000000000000 ) ) ;
#16264 = CARTESIAN_POINT ( 'NONE',  ( 4.999999999999999112, 9.314797388894893615, 5.239665997526921082 ) ) ;
#16265 = LINE ( 'NONE', #2095, #21583 ) ;
#16266 = VERTEX_POINT ( 'NONE', #1374 ) ;
#16267 = ORIENTED_EDGE ( 'NONE', *, *, #12877, .F. ) ;
#16268 = CARTESIAN_POINT ( 'NONE',  ( 1.520000000000000462, 1.010590785124388747E-15, 8.239200000000002078 ) ) ;
#16269 = VERTEX_POINT ( 'NONE', #8962 ) ;
#16270 = CARTESIAN_POINT ( 'NONE',  ( 58.50000000000000000, 12.82842712474617741, 12.17157287525379239 ) ) ;
#16271 = ORIENTED_EDGE ( 'NONE', *, *, #17458, .T. ) ;
#16272 = CARTESIAN_POINT ( 'NONE',  ( 0.000000000000000000, 0.000000000000000000, 3.059999999999998277 ) ) ;
#16273 = ORIENTED_EDGE ( 'NONE', *, *, #8663, .F. ) ;
#16274 = CARTESIAN_POINT ( 'NONE',  ( 54.09375000000000711, 11.65685424949236193, 10.99999999999998401 ) ) ;
#16275 = CIRCLE ( 'NONE', #21209, 8.265000000000021885 ) ;
#16276 = CARTESIAN_POINT ( 'NONE',  ( 69.20000000218495018, 12.50000000000000000, 14.99999999999999645 ) ) ;
#16277 = DIRECTION ( 'NONE',  ( 0.9396926207859107594, -0.3420201433256623291, 3.697785493223492838E-32 ) ) ;
#16278 = CARTESIAN_POINT ( 'NONE',  ( -68.64999999999999147, 7.499999999999996447, 16.03553390593273775 ) ) ;
#16279 = ADVANCED_FACE ( 'NONE', ( #14465 ), #7393, .T. ) ;
#16280 = CARTESIAN_POINT ( 'NONE',  ( 1.799999999999996048, 0.000000000000000000, 0.000000000000000000 ) ) ;
#16281 = VERTEX_POINT ( 'NONE', #23543 ) ;
#16282 = CARTESIAN_POINT ( 'NONE',  ( -2.828427124746188515, -2.828427124746190735, 18.25000000273119483 ) ) ;
#16283 = CARTESIAN_POINT ( 'NONE',  ( 45.00000000000000000, 15.00000000000001954, 10.00000000000008882 ) ) ;
#16284 = CARTESIAN_POINT ( 'NONE',  ( 59.77893183416158962, 8.411196891453236901, 10.97181229448535511 ) ) ;
#16285 = CARTESIAN_POINT ( 'NONE',  ( 1.709085384558223675, -3.079427455697027138, 2.039999999999996927 ) ) ;
#16286 = CARTESIAN_POINT ( 'NONE',  ( 68.25000000109245946, 9.999999999999998224, 17.06698730000000097 ) ) ;
#16287 = CARTESIAN_POINT ( 'NONE',  ( -20.00000000000000355, -8.499999999999966249, 2.449293598294706907E-15 ) ) ;
#16288 = EDGE_CURVE ( 'NONE', #14427, #9363, #4588, .T. ) ;
#16289 = CIRCLE ( 'NONE', #3645, 5.479999999999998650 ) ;
#16290 = CARTESIAN_POINT ( 'NONE',  ( -60.00000000000000711, -10.00000000000000178, 17.49999999999999645 ) ) ;
#16291 = ORIENTED_EDGE ( 'NONE', *, *, #2055, .T. ) ;
#16292 = DIRECTION ( 'NONE',  ( 0.000000000000000000, 0.000000000000000000, 1.000000000000000000 ) ) ;
#16293 = CARTESIAN_POINT ( 'NONE',  ( 54.46875000000000000, 6.999999999999992006, 13.75735931288071967 ) ) ;
#16294 = VECTOR ( 'NONE', #11975, 1000.000000000000000 ) ;
#16295 = CARTESIAN_POINT ( 'NONE',  ( 4.000000000000000000, 4.898587196589412829E-16, 0.9250000027311873207 ) ) ;
#16296 = CARTESIAN_POINT ( 'NONE',  ( -72.34999999999999432, 12.50000000000000000, 16.03553390593273775 ) ) ;
#16297 = ORIENTED_EDGE ( 'NONE', *, *, #9721, .F. ) ;
#16298 = DIRECTION ( 'NONE',  ( -1.000000000000000000, 0.000000000000000000, -0.000000000000000000 ) ) ;
#16299 = CARTESIAN_POINT ( 'NONE',  ( -2.117863837641485618E-16, 3.458734125000000326, -3.512499998634403209 ) ) ;
#16300 = DIRECTION ( 'NONE',  ( 0.000000000000000000, 0.000000000000000000, -1.000000000000000000 ) ) ;
#16301 = ORIENTED_EDGE ( 'NONE', *, *, #6277, .T. ) ;
#16302 = CARTESIAN_POINT ( 'NONE',  ( 69.79999999999999716, 11.76776695296636888, 13.23223304703362579 ) ) ;
#16303 = ORIENTED_EDGE ( 'NONE', *, *, #17898, .T. ) ;
#16304 = VECTOR ( 'NONE', #7900, 1000.000000000000000 ) ;
#16305 = VECTOR ( 'NONE', #13149, 1000.000000000000000 ) ;
#16306 = CYLINDRICAL_SURFACE ( 'NONE', #18270, 12.00000000000000000 ) ;
#16307 =( BOUNDED_SURFACE ( )  B_SPLINE_SURFACE ( 1, 2, ( 
 ( #13163, #20673, #9574, #5956, #4035, #15197, #11368, #18645, #11501, #9329, #554, #22461, #4278, #11611, #16621, #19810, #1487, #5446, #19929, #16127, #21843, #9298, #18377, #12891, #16585, #22060, #13012, #23648, #1720, #10756, #12781, #7263, #9061, #12673, #23412, #51, #12547, #23526, #3412, #11214, #10863, #21948, #8829, #11093, #14580, #18030, #7137, #1606, #7016, #20276, #8949, #16237, #21716, #14451, #16352, #20034, #5329, #7495, #3529, #3638, #1958, #14332, #164, #18140, #10975, #18251, #1836, #9187, #16473, #14811, #7384, #5677, #3880, #14692, #5561, #20147, #3751, #21595, #5207, #16702, #15285, #22669, #11338, #13597, #9889, #18962, #20863, #4117, #22557, #20513, #4244, #2544, #17183, #764, #4469, #11457, #6165, #18733, #11579, #8095, #6281, #18489, #5920, #2195, #22426, #18846, #2071, #278, #2432, #11691, #9412, #7613, #16830, #22189, #14935, #5803, #9764, #20391, #15167, #17063, #2322, #7736, #13487, #409, #13131, #523, #9655, #3998, #13366, #18608, #4354, #9532, #16945, #15406, #15052, #22308, #13249, #7843, #6039, #20635, #634, #7966, #20749, #7533, #11250, #13056, #1881, #1991, #87, #9447, #14497 ),
 ( #9226, #20312, #22103, #16624, #3913, #2110, #16742, #3677, #5484, #21760, #16509, #11014, #12819, #16394, #19851, #3802, #16282, #3567, #23574, #14978, #14616, #9334, #5245, #14849, #18298, #5371, #10903, #7182, #12589, #323, #12713, #19965, #1764, #18182, #20077, #7420, #9102, #18525, #23692, #14731, #5724, #10793, #7655, #21877, #7308, #21990, #5604, #12930, #20193, #3456, #11140, #18068, #1648, #18414, #202, #8992, #998, #15649, #4038, #20429, #19320, #3035, #15091, #17667, #8330, #22920, #22230, #16871, #10256, #1228, #13851, #5839, #6532, #8566, #21106, #17432, #6648, #12054, #4721, #23037, #1113, #21220, #11371, #13961, #18648, #20552, #2909, #8459, #558, #19210, #9578, #17550, #15766, #13166, #2798, #447, #2237, #7772, #22346, #10382, #5959, #13285, #4158, #4835, #12166, #19437, #11505, #11945, #18776, #2357, #20676, #9689, #16985, #7882, #15200, #22465, #6077, #13409, #4609, #10140, #21825, #23632, #12530, #12651, #10737, #20017, #1347, #5311, #14561, #19911, #16109, #6760, #18123, #5072, #8683, #15874, #10495, #18236, #14076, #16221, #12765, #1819, #3619, #17776, #21700, #15984, #10959, #19556, #23393, #8811, #19792 ) ),
 .UNSPECIFIED., .F., .F., .F. ) 
 B_SPLINE_SURFACE_WITH_KNOTS ( ( 2, 2 ),
 ( 3, 2, 2, 2, 2, 2, 2, 2, 2, 2, 2, 2, 2, 2, 2, 2, 2, 2, 2, 2, 2, 2, 2, 2, 2, 2, 2, 2, 2, 2, 2, 2, 2, 2, 2, 2, 2, 2, 2, 2, 2, 2, 2, 2, 2, 2, 2, 2, 2, 2, 2, 2, 2, 2, 2, 2, 2, 2, 2, 2, 2, 2, 2, 2, 2, 2, 2, 2, 2, 2, 2, 2, 2, 2, 2, 3 ),
 ( 0.000000000000000000, 1.000000000000000000 ),
 ( -0.009250000000000001277, 0.000000000000000000, 0.01250000000000000069, 0.02500000000000000139, 0.03749999999999999861, 0.05000000000000000278, 0.06250000000000000000, 0.07499999999999999722, 0.08749999999999999445, 0.1000000000000000056, 0.1125000000000000028, 0.1250000000000000000, 0.1375000000000000111, 0.1499999999999999944, 0.1625000000000000056, 0.1749999999999999889, 0.1875000000000000000, 0.2000000000000000111, 0.2124999999999999944, 0.2250000000000000056, 0.2374999999999999889, 0.2500000000000000000, 0.2625000000000000111, 0.2750000000000000222, 0.2874999999999999778, 0.2999999999999999889, 0.3125000000000000000, 0.3250000000000000111, 0.3375000000000000222, 0.3499999999999999778, 0.3624999999999999889, 0.3750000000000000000, 0.3875000000000000111, 0.4000000000000000222, 0.4124999999999999778, 0.4249999999999999889, 0.4375000000000000000, 0.4500000000000000111, 0.4625000000000000222, 0.4749999999999999778, 0.4874999999999999889, 0.5000000000000000000, 0.5124999999999999556, 0.5250000000000000222, 0.5374999999999999778, 0.5500000000000000444, 0.5625000000000000000, 0.5749999999999999556, 0.5875000000000000222, 0.5999999999999999778, 0.6125000000000000444, 0.6250000000000000000, 0.6374999999999999556, 0.6500000000000000222, 0.6624999999999999778, 0.6750000000000000444, 0.6875000000000000000, 0.6999999999999999556, 0.7125000000000000222, 0.7249999999999999778, 0.7375000000000000444, 0.7500000000000000000, 0.7624999999999999556, 0.7750000000000000222, 0.7874999999999999778, 0.8000000000000000444, 0.8125000000000000000, 0.8249999999999999556, 0.8375000000000000222, 0.8499999999999999778, 0.8625000000000000444, 0.8750000000000000000, 0.8874999999999999556, 0.9000000000000000222, 0.9124999999999999778, 0.9250000000000000444 ),
 .UNSPECIFIED. ) 
 GEOMETRIC_REPRESENTATION_ITEM ( )  RATIONAL_B_SPLINE_SURFACE ( (
 ( 1.000000000000000000, 1.000000000000000000, 1.000000000000000000, 0.9238795325112867385, 1.000000000000000000, 0.9238795325112867385, 1.000000000000000000, 0.9238795325112867385, 1.000000000000000000, 0.9238795325112867385, 1.000000000000000000, 0.9238795325112867385, 1.000000000000000000, 0.9238795325112867385, 1.000000000000000000, 0.9238795325112867385, 1.000000000000000000, 0.9238795325112867385, 1.000000000000000000, 0.9238795325112867385, 1.000000000000000000, 0.9238795325112867385, 1.000000000000000000, 0.9238795325112867385, 1.000000000000000000, 0.9238795325112867385, 1.000000000000000000, 0.9238795325112867385, 1.000000000000000000, 0.9238795325112867385, 1.000000000000000000, 0.9238795325112867385, 1.000000000000000000, 0.9238795325112867385, 1.000000000000000000, 0.9238795325112867385, 1.000000000000000000, 0.9238795325112867385, 1.000000000000000000, 0.9238795325112867385, 1.000000000000000000, 0.9238795325112867385, 1.000000000000000000, 0.9238795325112867385, 1.000000000000000000, 0.9238795325112867385, 1.000000000000000000, 0.9238795325112867385, 1.000000000000000000, 0.9238795325112867385, 1.000000000000000000, 0.9238795325112867385, 1.000000000000000000, 0.9238795325112867385, 1.000000000000000000, 0.9238795325112867385, 1.000000000000000000, 0.9238795325112867385, 1.000000000000000000, 0.9238795325112867385, 1.000000000000000000, 0.9238795325112867385, 1.000000000000000000, 0.9238795325112867385, 1.000000000000000000, 0.9238795325112867385, 1.000000000000000000, 0.9238795325112867385, 1.000000000000000000, 0.9238795325112867385, 1.000000000000000000, 0.9238795325112867385, 1.000000000000000000, 0.9238795325112867385, 1.000000000000000000, 0.9238795325112867385, 1.000000000000000000, 0.9238795325112867385, 1.000000000000000000, 0.9238795325112867385, 1.000000000000000000, 0.9238795325112867385, 1.000000000000000000, 0.9238795325112867385, 1.000000000000000000, 0.9238795325112867385, 1.000000000000000000, 0.9238795325112867385, 1.000000000000000000, 0.9238795325112867385, 1.000000000000000000, 0.9238795325112867385, 1.000000000000000000, 0.9238795325112867385, 1.000000000000000000, 0.9238795325112867385, 1.000000000000000000, 0.9238795325112867385, 1.000000000000000000, 0.9238795325112867385, 1.000000000000000000, 0.9238795325112867385, 1.000000000000000000, 0.9238795325112867385, 1.000000000000000000, 0.9238795325112867385, 1.000000000000000000, 0.9238795325112867385, 1.000000000000000000, 0.9238795325112867385, 1.000000000000000000, 0.9238795325112867385, 1.000000000000000000, 0.9238795325112867385, 1.000000000000000000, 0.9238795325112867385, 1.000000000000000000, 0.9238795325112867385, 1.000000000000000000, 0.9238795325112867385, 1.000000000000000000, 0.9238795325112867385, 1.000000000000000000, 0.9238795325112867385, 1.000000000000000000, 0.9238795325112867385, 1.000000000000000000, 0.9238795325112867385, 1.000000000000000000, 0.9238795325112867385, 1.000000000000000000, 0.9238795325112867385, 1.000000000000000000, 0.9238795325112867385, 1.000000000000000000, 0.9238795325112867385, 1.000000000000000000, 0.9238795325112867385, 1.000000000000000000, 0.9238795325112867385, 1.000000000000000000, 0.9238795325112867385, 1.000000000000000000, 0.9238795325112867385, 1.000000000000000000, 0.9238795325112867385, 1.000000000000000000, 0.9238795325112867385, 1.000000000000000000, 0.9238795325112867385, 1.000000000000000000),
 ( 1.000000000000000000, 1.000000000000000000, 1.000000000000000000, 0.9238795325112867385, 1.000000000000000000, 0.9238795325112867385, 1.000000000000000000, 0.9238795325112867385, 1.000000000000000000, 0.9238795325112867385, 1.000000000000000000, 0.9238795325112867385, 1.000000000000000000, 0.9238795325112867385, 1.000000000000000000, 0.9238795325112867385, 1.000000000000000000, 0.9238795325112867385, 1.000000000000000000, 0.9238795325112867385, 1.000000000000000000, 0.9238795325112867385, 1.000000000000000000, 0.9238795325112867385, 1.000000000000000000, 0.9238795325112867385, 1.000000000000000000, 0.9238795325112867385, 1.000000000000000000, 0.9238795325112867385, 1.000000000000000000, 0.9238795325112867385, 1.000000000000000000, 0.9238795325112867385, 1.000000000000000000, 0.9238795325112867385, 1.000000000000000000, 0.9238795325112867385, 1.000000000000000000, 0.9238795325112867385, 1.000000000000000000, 0.9238795325112867385, 1.000000000000000000, 0.9238795325112867385, 1.000000000000000000, 0.9238795325112867385, 1.000000000000000000, 0.9238795325112867385, 1.000000000000000000, 0.9238795325112867385, 1.000000000000000000, 0.9238795325112867385, 1.000000000000000000, 0.9238795325112867385, 1.000000000000000000, 0.9238795325112867385, 1.000000000000000000, 0.9238795325112867385, 1.000000000000000000, 0.9238795325112867385, 1.000000000000000000, 0.9238795325112867385, 1.000000000000000000, 0.9238795325112867385, 1.000000000000000000, 0.9238795325112867385, 1.000000000000000000, 0.9238795325112867385, 1.000000000000000000, 0.9238795325112867385, 1.000000000000000000, 0.9238795325112867385, 1.000000000000000000, 0.9238795325112867385, 1.000000000000000000, 0.9238795325112867385, 1.000000000000000000, 0.9238795325112867385, 1.000000000000000000, 0.9238795325112867385, 1.000000000000000000, 0.9238795325112867385, 1.000000000000000000, 0.9238795325112867385, 1.000000000000000000, 0.9238795325112867385, 1.000000000000000000, 0.9238795325112867385, 1.000000000000000000, 0.9238795325112867385, 1.000000000000000000, 0.9238795325112867385, 1.000000000000000000, 0.9238795325112867385, 1.000000000000000000, 0.9238795325112867385, 1.000000000000000000, 0.9238795325112867385, 1.000000000000000000, 0.9238795325112867385, 1.000000000000000000, 0.9238795325112867385, 1.000000000000000000, 0.9238795325112867385, 1.000000000000000000, 0.9238795325112867385, 1.000000000000000000, 0.9238795325112867385, 1.000000000000000000, 0.9238795325112867385, 1.000000000000000000, 0.9238795325112867385, 1.000000000000000000, 0.9238795325112867385, 1.000000000000000000, 0.9238795325112867385, 1.000000000000000000, 0.9238795325112867385, 1.000000000000000000, 0.9238795325112867385, 1.000000000000000000, 0.9238795325112867385, 1.000000000000000000, 0.9238795325112867385, 1.000000000000000000, 0.9238795325112867385, 1.000000000000000000, 0.9238795325112867385, 1.000000000000000000, 0.9238795325112867385, 1.000000000000000000, 0.9238795325112867385, 1.000000000000000000, 0.9238795325112867385, 1.000000000000000000, 0.9238795325112867385, 1.000000000000000000, 0.9238795325112867385, 1.000000000000000000, 0.9238795325112867385, 1.000000000000000000, 0.9238795325112867385, 1.000000000000000000, 0.9238795325112867385, 1.000000000000000000, 0.9238795325112867385, 1.000000000000000000, 0.9238795325112867385, 1.000000000000000000, 0.9238795325112867385, 1.000000000000000000) ) ) 
 REPRESENTATION_ITEM ( '' )  SURFACE ( )  );
#16308 = CARTESIAN_POINT ( 'NONE',  ( 4.000000000000000888, 4.898587196589412829E-16, 19.50000000000001066 ) ) ;
#16309 = DIRECTION ( 'NONE',  ( -1.000000000000000000, -3.552713678800500929E-15, 0.000000000000000000 ) ) ;
#16310 = DIRECTION ( 'NONE',  ( 1.000000000000000000, 0.000000000000000000, 0.000000000000000000 ) ) ;
#16311 = DIRECTION ( 'NONE',  ( 0.000000000000000000, -1.000000000000000000, -1.040834085586083783E-14 ) ) ;
#16312 = CARTESIAN_POINT ( 'NONE',  ( -66.19999999999998863, 8.232233047033627571, 16.76776695296636532 ) ) ;
#16313 = DIRECTION ( 'NONE',  ( 1.000000000000000000, 0.000000000000000000, 0.000000000000000000 ) ) ;
#16314 = EDGE_CURVE ( 'NONE', #4004, #4847, #2216, .T. ) ;
#16315 = CARTESIAN_POINT ( 'NONE',  ( 1.432654583217643163, -3.458734124999999437, 16.75000000136560629 ) ) ;
#16316 = CYLINDRICAL_SURFACE ( 'NONE', #18744, 4.000000000000000000 ) ;
#16317 = CARTESIAN_POINT ( 'NONE',  ( 2.828427124746189847, 2.828427124746190291, 3.925000000000002931 ) ) ;
#16318 = PLANE ( 'NONE',  #11707 ) ;
#16319 = CARTESIAN_POINT ( 'NONE',  ( 68.35000000218495586, 12.50000000000000000, 13.96446609406725692 ) ) ;
#16320 = CARTESIAN_POINT ( 'NONE',  ( 2.445694354108821411, 2.445694354108820523, 16.06250000136560629 ) ) ;
#16321 = CARTESIAN_POINT ( 'NONE',  ( 4.999999999999999112, 3.174628368996190719, -8.152713396088728359 ) ) ;
#16322 = VERTEX_POINT ( 'NONE', #3427 ) ;
#16323 = CARTESIAN_POINT ( 'NONE',  ( -68.20000000109246230, 7.933012699999995476, 15.85617417291294196 ) ) ;
#16324 = VERTEX_POINT ( 'NONE', #17806 ) ;
#16325 = CARTESIAN_POINT ( 'NONE',  ( 56.40393183416158251, 14.02818770551463956, 13.41119689145323335 ) ) ;
#16326 = CARTESIAN_POINT ( 'NONE',  ( -67.85000000109248219, 12.06698730000000097, 14.99999999999999645 ) ) ;
#16327 = CARTESIAN_POINT ( 'NONE',  ( -3.458734125000000326, 0.000000000000000000, -2.262499998634403653 ) ) ;
#16328 = ORIENTED_EDGE ( 'NONE', *, *, #4855, .F. ) ;
#16329 = ORIENTED_EDGE ( 'NONE', *, *, #22423, .F. ) ;
#16330 = FACE_OUTER_BOUND ( 'NONE', #15730, .T. ) ;
#16331 = CARTESIAN_POINT ( 'NONE',  ( 60.00000000000000711, 12.12132034355963484, 12.87867965644034740 ) ) ;
#16332 = CARTESIAN_POINT ( 'NONE',  ( -65.50000000218494733, 8.232233047033627571, 16.76776695296636532 ) ) ;
#16333 = AXIS2_PLACEMENT_3D ( 'NONE', #5401, #18211, #9137 ) ;
#16334 = CARTESIAN_POINT ( 'NONE',  ( -69.35000000109246798, 8.538419263543524096, 13.53841926354352054 ) ) ;
#16335 = CARTESIAN_POINT ( 'NONE',  ( -2.445694354108819191, 2.445694354108820523, 13.56250000136560629 ) ) ;
#16336 = CARTESIAN_POINT ( 'NONE',  ( 6.405354440716562792, -8.974600000000002353, 5.000000000000079936 ) ) ;
#16337 = CARTESIAN_POINT ( 'NONE',  ( 60.52893183416158251, 11.17458954617365663, 18.02818770551464311 ) ) ;
#16338 = CARTESIAN_POINT ( 'NONE',  ( 4.999999999999999112, 0.000000000000000000, 0.000000000000000000 ) ) ;
#16339 = CARTESIAN_POINT ( 'NONE',  ( 56.06250000000000000, 6.999999999999997335, 15.00000000000000533 ) ) ;
#16340 = CARTESIAN_POINT ( 'NONE',  ( -3.999999999999999112, 1.656854249492380804, 19.06250000273119483 ) ) ;
#16341 = DIRECTION ( 'NONE',  ( -0.000000000000000000, 0.000000000000000000, -1.000000000000000000 ) ) ;
#16342 = VECTOR ( 'NONE', #13931, 1000.000000000000114 ) ;
#16343 = VERTEX_POINT ( 'NONE', #18265 ) ;
#16344 = DIRECTION ( 'NONE',  ( 1.000000000000000000, 7.703719777548943412E-32, 0.000000000000000000 ) ) ;
#16345 = CARTESIAN_POINT ( 'NONE',  ( -10.00000000000000000, 0.000000000000000000, 0.000000000000000000 ) ) ;
#16346 = VERTEX_POINT ( 'NONE', #16252 ) ;
#16347 = CARTESIAN_POINT ( 'NONE',  ( 54.93750000000000711, 10.00000000000000711, 17.99999999999999645 ) ) ;
#16348 = SURFACE_SIDE_STYLE ('',( #1832 ) ) ;
#16349 = CARTESIAN_POINT ( 'NONE',  ( 7.347880794884118750E-16, -4.000000000000000000, -2.324999997268812013 ) ) ;
#16350 = DIRECTION ( 'NONE',  ( -4.930380657631312836E-32, -0.3420201433256691015, -0.9396926207859083169 ) ) ;
#16351 = EDGE_LOOP ( 'NONE', ( #13396, #5172, #11479, #695 ) ) ;
#16352 = CARTESIAN_POINT ( 'NONE',  ( 9.920644283265380691E-16, 4.000000000000000000, 16.75000000000001066 ) ) ;
#16353 = ORIENTED_EDGE ( 'NONE', *, *, #3448, .T. ) ;
#16354 = ADVANCED_FACE ( 'NONE', ( #14592 ), #5343, .F. ) ;
#16355 = CARTESIAN_POINT ( 'NONE',  ( -1.647987302177966740E-14, -7.505553499465137612, -0.5805565836007695601 ) ) ;
#16356 = DIRECTION ( 'NONE',  ( -1.000000000000000000, 0.000000000000000000, -0.000000000000000000 ) ) ;
#16357 = ORIENTED_EDGE ( 'NONE', *, *, #19256, .T. ) ;
#16358 = DIRECTION ( 'NONE',  ( 0.000000000000000000, 0.000000000000000000, -1.000000000000000000 ) ) ;
#16359 = CARTESIAN_POINT ( 'NONE',  ( -2.100000000000000089, 2.571758278209441957E-16, -4.694516984716113228 ) ) ;
#16360 = EDGE_CURVE ( 'NONE', #7647, #5505, #6223, .T. ) ;
#16361 = CARTESIAN_POINT ( 'NONE',  ( 7.829898480332751376, -11.25000000000000355, 10.00000000000008882 ) ) ;
#16362 = PRESENTATION_LAYER_ASSIGNMENT (  '', '', ( #4480 ) ) ;
#16363 = CONICAL_SURFACE ( 'NONE', #17131, 2.500000000000000888, 0.9599310885968785900 ) ;
#16364 = CARTESIAN_POINT ( 'NONE',  ( 72.05000000000001137, 8.964466094067258695, 12.49999999999999289 ) ) ;
#16365 = PLANE ( 'NONE',  #13930 ) ;
#16366 = DIRECTION ( 'NONE',  ( 1.224646799147353207E-16, 0.000000000000000000, 1.000000000000000000 ) ) ;
#16367 = CARTESIAN_POINT ( 'NONE',  ( 54.31481816583844591, 14.00000000000000178, 14.93194885905434610 ) ) ;
#16368 = CARTESIAN_POINT ( 'NONE',  ( -1.432654583217640942, -3.458734124999999882, -0.07499999863440427739 ) ) ;
#16369 =( LENGTH_UNIT ( ) NAMED_UNIT ( * ) SI_UNIT ( .MILLI., .METRE. ) );
#16370 = CARTESIAN_POINT ( 'NONE',  ( 2.828427124746189847, 2.828427124746190291, -0.07499999999999867883 ) ) ;
#16371 = CIRCLE ( 'NONE', #4497, 8.749000000000002331 ) ;
#16372 = DIRECTION ( 'NONE',  ( 0.000000000000000000, 0.000000000000000000, -1.000000000000000000 ) ) ;
#16373 = VERTEX_POINT ( 'NONE', #23307 ) ;
#16374 = CARTESIAN_POINT ( 'NONE',  ( 6.499999999999999112, -1.264206540070616835, -3.645490429492275197 ) ) ;
#16375 = CARTESIAN_POINT ( 'NONE',  ( 0.000000000000000000, 0.000000000000000000, -4.000000000000000000 ) ) ;
#16376 = FACE_OUTER_BOUND ( 'NONE', #19124, .T. ) ;
#16377 = ORIENTED_EDGE ( 'NONE', *, *, #20093, .F. ) ;
#16378 = VECTOR ( 'NONE', #2546, 1000.000000000000000 ) ;
#16379 = ORIENTED_EDGE ( 'NONE', *, *, #12738, .T. ) ;
#16380 = ADVANCED_FACE ( 'NONE', ( #17921 ), #23425, .F. ) ;
#16381 = DIRECTION ( 'NONE',  ( -1.000000000000000000, -0.000000000000000000, -0.000000000000000000 ) ) ;
#16382 = EDGE_CURVE ( 'NONE', #14730, #14629, #10646, .T. ) ;
#16383 = CARTESIAN_POINT ( 'NONE',  ( 57.84375000000000711, 8.343145750507636293, 19.00000000000000000 ) ) ;
#16384 = VERTEX_POINT ( 'NONE', #9075 ) ;
#16385 = CARTESIAN_POINT ( 'NONE',  ( 51.00000000000000711, 12.47487373415290612, 12.52512626584706901 ) ) ;
#16386 = ORIENTED_EDGE ( 'NONE', *, *, #22195, .T. ) ;
#16387 = CARTESIAN_POINT ( 'NONE',  ( 56.93981816583843170, 10.06805114094564857, 19.00000000000000000 ) ) ;
#16388 = EDGE_CURVE ( 'NONE', #6601, #9734, #3650, .T. ) ;
#16389 = CARTESIAN_POINT ( 'NONE',  ( 69.00000000218494733, 9.999999999999998224, 12.49999999999999289 ) ) ;
#16390 = DIRECTION ( 'NONE',  ( 0.000000000000000000, -0.7071067811865414665, 0.7071067811865536790 ) ) ;
#16391 = DIRECTION ( 'NONE',  ( -1.000000000000000000, 0.000000000000000000, 1.224646799147353207E-16 ) ) ;
#16392 = CARTESIAN_POINT ( 'NONE',  ( 4.000000000000000888, -1.656854249492379694, -0.2624999999999966804 ) ) ;
#16393 = ORIENTED_EDGE ( 'NONE', *, *, #9232, .F. ) ;
#16394 = CARTESIAN_POINT ( 'NONE',  ( 1.656854249492384135, -3.999999999999999112, 18.43750000273119483 ) ) ;
#16395 = CIRCLE ( 'NONE', #11444, 0.2500000000000002220 ) ;
#16396 = DIRECTION ( 'NONE',  ( 1.000000000000000000, 0.000000000000000000, 0.000000000000000000 ) ) ;
#16397 = CARTESIAN_POINT ( 'NONE',  ( 60.43518183416157541, 9.931948859054379852, 18.99999999999999289 ) ) ;
#16398 = CARTESIAN_POINT ( 'NONE',  ( 3.596871450741750742, 1.575092265385753310, 2.039999999999997815 ) ) ;
#16399 = DIRECTION ( 'NONE',  ( 1.000000000000000000, 0.000000000000000000, 0.000000000000000000 ) ) ;
#16400 = CARTESIAN_POINT ( 'NONE',  ( -69.29999999999999716, 9.999999999999998224, 17.49999999999999645 ) ) ;
#16401 = CARTESIAN_POINT ( 'NONE',  ( 8.718769219667262149, -11.25000000000000355, 5.000000000000079936 ) ) ;
#16402 = ORIENTED_EDGE ( 'NONE', *, *, #1994, .T. ) ;
#16403 = PLANE ( 'NONE',  #3948 ) ;
#16404 = CARTESIAN_POINT ( 'NONE',  ( 57.75000000000000000, 7.878679656440361612, 17.12132034355964549 ) ) ;
#16405 = EDGE_CURVE ( 'NONE', #11298, #20452, #6916, .T. ) ;
#16406 = DIRECTION ( 'NONE',  ( 1.000000000000000000, 0.000000000000000000, 0.000000000000000000 ) ) ;
#16407 = VECTOR ( 'NONE', #13825, 1000.000000000000114 ) ;
#16408 = EDGE_LOOP ( 'NONE', ( #15760, #1891, #22709 ) ) ;
#16409 = VECTOR ( 'NONE', #6175, 1000.000000000000000 ) ;
#16410 = DIRECTION ( 'NONE',  ( 0.000000000000000000, 0.000000000000000000, -1.000000000000000000 ) ) ;
#16411 = DIRECTION ( 'NONE',  ( 0.000000000000000000, 0.000000000000000000, -1.000000000000000000 ) ) ;
#16412 = LINE ( 'NONE', #12950, #10167 ) ;
#16413 = EDGE_CURVE ( 'NONE', #17247, #16102, #12644, .T. ) ;
#16414 = ORIENTED_EDGE ( 'NONE', *, *, #14406, .T. ) ;
#16415 = CARTESIAN_POINT ( 'NONE',  ( 4.000000000000000888, 4.898587196589412829E-16, 19.50000000000001066 ) ) ;
#16416 = VERTEX_POINT ( 'NONE', #12901 ) ;
#16417 = CARTESIAN_POINT ( 'NONE',  ( -1.600000000000004086, 0.000000000000000000, 0.000000000000000000 ) ) ;
#16418 = AXIS2_PLACEMENT_3D ( 'NONE', #12580, #14487, #14721 ) ;
#16419 = CARTESIAN_POINT ( 'NONE',  ( 1.025207404391860050E-15, 3.458734125000000770, 10.43750000136560629 ) ) ;
#16420 = EDGE_CURVE ( 'NONE', #5838, #2784, #14233, .T. ) ;
#16421 = CARTESIAN_POINT ( 'NONE',  ( -66.29999999999999716, 7.499999999999996447, 14.99999999999999645 ) ) ;
#16422 = EDGE_CURVE ( 'NONE', #1978, #8665, #21014, .T. ) ;
#16423 = CIRCLE ( 'NONE', #17573, 2.649999999999999467 ) ;
#16424 = DIRECTION ( 'NONE',  ( -1.000000000000000000, 0.000000000000000000, 0.000000000000000000 ) ) ;
#16425 = VECTOR ( 'NONE', #20818, 1000.000000000000000 ) ;
#16426 = CARTESIAN_POINT ( 'NONE',  ( -66.99999999999998579, 8.232233047033627571, 16.76776695296636532 ) ) ;
#16427 = CARTESIAN_POINT ( 'NONE',  ( 4.999999999999999112, 3.174628368996077477, 8.152713396088774545 ) ) ;
#16428 = CARTESIAN_POINT ( 'NONE',  ( -3.458734124999998993, 0.000000000000000000, 19.43750000136560629 ) ) ;
#16429 = DIRECTION ( 'NONE',  ( 0.000000000000000000, 0.000000000000000000, 1.000000000000000000 ) ) ;
#16430 = MECHANICAL_DESIGN_GEOMETRIC_PRESENTATION_REPRESENTATION (  '', ( #1876 ), #20235 ) ;
#16431 = CIRCLE ( 'NONE', #730, 4.000000000000001776 ) ;
#16432 = CARTESIAN_POINT ( 'NONE',  ( -4.000000000000000000, 0.000000000000000000, 6.300000000000001599 ) ) ;
#16433 = CARTESIAN_POINT ( 'NONE',  ( -0.7060087303327398089, -11.25000000000000355, 5.000000000000079936 ) ) ;
#16434 = CARTESIAN_POINT ( 'NONE',  ( 1.432654583217643163, -3.458734124999999437, 14.75000000136560452 ) ) ;
#16435 = CARTESIAN_POINT ( 'NONE',  ( 49.55947366966726264, -11.25000000000000355, 5.000000000000079936 ) ) ;
#16436 = VERTEX_POINT ( 'NONE', #1967 ) ;
#16437 = CARTESIAN_POINT ( 'NONE',  ( -68.95000000109247651, 8.538419263543522320, 16.46158073645647235 ) ) ;
#16438 = VERTEX_POINT ( 'NONE', #20403 ) ;
#16439 = CARTESIAN_POINT ( 'NONE',  ( 54.06018183416157541, 5.999999999999996447, 14.93194885905437808 ) ) ;
#16440 = CARTESIAN_POINT ( 'NONE',  ( -66.05000000109247082, 9.999999999999998224, 12.93301269999999192 ) ) ;
#16441 = CARTESIAN_POINT ( 'NONE',  ( 27.50000000000000000, 12.50000000000000178, -33.66025403784446723 ) ) ;
#16442 =( BOUNDED_CURVE ( )  B_SPLINE_CURVE ( 2, ( #18468, #6988, #21567, #20252, #3858, #10728, #14428, #16448, #11068 ),
 .UNSPECIFIED., .F., .F. ) 
 B_SPLINE_CURVE_WITH_KNOTS ( ( 3, 2, 2, 2, 3 ),
 ( 0.1875000000000010270, 0.2031250000000009437, 0.2187500000000008327, 0.2343750000000007494, 0.2500000000000006661 ),
 .UNSPECIFIED. ) 
 CURVE ( )  GEOMETRIC_REPRESENTATION_ITEM ( )  RATIONAL_B_SPLINE_CURVE ( ( 0.9999999999999950040, 0.9238795325112917345, 1.000000000000000000, 0.9238795325112867385, 1.000000000000000000, 0.9238795325112867385, 1.000000000000000000, 0.9238795325112835188, 1.000000000000003331 ) ) 
 REPRESENTATION_ITEM ( '' )  );
#16443 = AXIS2_PLACEMENT_3D ( 'NONE', #13662, #1280, #8271 ) ;
#16444 = CARTESIAN_POINT ( 'NONE',  ( -60.00000000000000711, 15.00000000000000000, 25.00000000000001421 ) ) ;
#16445 = ORIENTED_EDGE ( 'NONE', *, *, #12422, .F. ) ;
#16446 = CIRCLE ( 'NONE', #12258, 8.749000000000000554 ) ;
#16447 = ORIENTED_EDGE ( 'NONE', *, *, #10439, .F. ) ;
#16448 = CARTESIAN_POINT ( 'NONE',  ( 70.95000000000000284, 8.964466094067294222, 17.50000000000003908 ) ) ;
#16449 = EDGE_CURVE ( 'NONE', #402, #16416, #10349, .T. ) ;
#16450 = CARTESIAN_POINT ( 'NONE',  ( 51.87731816583844591, 7.830560233210212218, 12.92679907967049679 ) ) ;
#16451 = EDGE_CURVE ( 'NONE', #23288, #10547, #2207, .T. ) ;
#16452 = CARTESIAN_POINT ( 'NONE',  ( -69.50000000109248788, 12.06698730000000275, 15.85617417291294196 ) ) ;
#16453 = AXIS2_PLACEMENT_3D ( 'NONE', #15424, #6299, #20878 ) ;
#16454 = CARTESIAN_POINT ( 'NONE',  ( -69.45000000109247651, 9.999999999999998224, 12.93301269999999192 ) ) ;
#16455 = CARTESIAN_POINT ( 'NONE',  ( -2.445694354108819191, 2.445694354108820523, 11.56250000136560629 ) ) ;
#16456 = CARTESIAN_POINT ( 'NONE',  ( 2.500000000000000000, -2.357898499370432166, 3.035766082959412415E-15 ) ) ;
#16457 = CARTESIAN_POINT ( 'NONE',  ( 55.21875000000000000, 13.00000000000000711, 16.24264068711927322 ) ) ;
#16458 = CARTESIAN_POINT ( 'NONE',  ( -60.00000000000000711, -9.999999999999998224, 25.00000000000001421 ) ) ;
#16459 = AXIS2_PLACEMENT_3D ( 'NONE', #1702, #9046, #23507 ) ;
#16460 = CARTESIAN_POINT ( 'NONE',  ( 51.18750000000000711, 9.999999999999989342, 11.99999999999999467 ) ) ;
#16461 = CARTESIAN_POINT ( 'NONE',  ( 1.971781867644420635E-15, -4.000000000000000000, 17.37500000273119483 ) ) ;
#16462 = DIRECTION ( 'NONE',  ( -1.000000000000000000, -0.000000000000000000, 0.000000000000000000 ) ) ;
#16463 = EDGE_LOOP ( 'NONE', ( #2350, #22758, #19981, #16117 ) ) ;
#16464 = CARTESIAN_POINT ( 'NONE',  ( 70.20000000000000284, 8.232233047033627571, 16.76776695296636532 ) ) ;
#16465 = DIRECTION ( 'NONE',  ( 0.000000000000000000, 0.000000000000000000, -1.000000000000000000 ) ) ;
#16466 = ORIENTED_EDGE ( 'NONE', *, *, #7337, .T. ) ;
#16467 = CARTESIAN_POINT ( 'NONE',  ( 56.25000000000000711, 7.878679656440361612, 17.12132034355964549 ) ) ;
#16469 = AXIS2_PLACEMENT_3D ( 'NONE', #2776, #977, #4700 ) ;
#16468 = FILL_AREA_STYLE_COLOUR ( '', #6450 ) ;
#16470 = CARTESIAN_POINT ( 'NONE',  ( 4.000000000000000000, 1.656854249492381248, -3.012499997268812457 ) ) ;
#16471 = CARTESIAN_POINT ( 'NONE',  ( 9.920644283265380691E-16, 4.000000000000000000, 9.875000002731196602 ) ) ;
#16472 = EDGE_LOOP ( 'NONE', ( #23649, #19050, #8606, #1956 ) ) ;
#16473 = CARTESIAN_POINT ( 'NONE',  ( -2.828427124746189403, 2.828427124746190291, 15.87500000000001066 ) ) ;
#16474 = FACE_OUTER_BOUND ( 'NONE', #18898, .T. ) ;
#16475 = EDGE_LOOP ( 'NONE', ( #7375, #13588, #20121, #20536 ) ) ;
#16476 = DIRECTION ( 'NONE',  ( 1.000000000000000000, 0.000000000000000000, -9.637352644315595243E-17 ) ) ;
#16477 = CARTESIAN_POINT ( 'NONE',  ( 1.125461230421587633, -3.270501301980698550, 2.040000000000001812 ) ) ;
#16478 = CARTESIAN_POINT ( 'NONE',  ( 2.445694354108820967, -2.445694354108820079, -0.6374999986344023206 ) ) ;
#16479 = VECTOR ( 'NONE', #4419, 1000.000000000000114 ) ;
#16480 =( GEOMETRIC_REPRESENTATION_CONTEXT ( 3 ) GLOBAL_UNCERTAINTY_ASSIGNED_CONTEXT ( ( #3062 ) ) GLOBAL_UNIT_ASSIGNED_CONTEXT ( ( #21533, #1542, #5260 ) ) REPRESENTATION_CONTEXT ( 'NONE', 'WORKASPACE' ) );
#16481 = CARTESIAN_POINT ( 'NONE',  ( 69.05000000000002558, 12.50000000000000000, 13.96446609406725869 ) ) ;
#16482 = PRODUCT_RELATED_PRODUCT_CATEGORY ( 'part', '', ( #16983 ) ) ;
#16483 = DIRECTION ( 'NONE',  ( -0.8660254037844377084, -0.5000000000000015543, 0.000000000000000000 ) ) ;
#16484 = EDGE_CURVE ( 'NONE', #11881, #14277, #16597, .T. ) ;
#16485 = DIRECTION ( 'NONE',  ( -0.000000000000000000, -1.000000000000000000, -0.000000000000000000 ) ) ;
#16486 = CARTESIAN_POINT ( 'NONE',  ( 53.93981816583844591, 10.06805114094564857, 19.00000000000000000 ) ) ;
#16487 = CARTESIAN_POINT ( 'NONE',  ( 2.445694354108820079, 2.445694354108820523, 1.362500001365595903 ) ) ;
#16488 = CARTESIAN_POINT ( 'NONE',  ( 1.872352939448454495E-15, -3.458734125000000326, 10.68750000136560452 ) ) ;
#16489 = DIRECTION ( 'NONE',  ( -1.000000000000000000, -7.703719777548943412E-32, 0.000000000000000000 ) ) ;
#16490 = CARTESIAN_POINT ( 'NONE',  ( 2.828427124746192067, -2.828427124746189847, 18.50000000273119483 ) ) ;
#16491 = DIRECTION ( 'NONE',  ( 0.000000000000000000, 0.000000000000000000, 1.000000000000000000 ) ) ;
#16492 = ORIENTED_EDGE ( 'NONE', *, *, #19256, .F. ) ;
#16493 = CARTESIAN_POINT ( 'NONE',  ( -0.04760896646565748735, 3.990996980104895897, 2.039999999999998259 ) ) ;
#16494 = CARTESIAN_POINT ( 'NONE',  ( 0.000000000000000000, 0.000000000000000000, 0.000000000000000000 ) ) ;
#16495 = DIRECTION ( 'NONE',  ( -1.000000000000000000, -7.703719777548943412E-32, 0.000000000000000000 ) ) ;
#16496 = VECTOR ( 'NONE', #13448, 1000.000000000000000 ) ;
#16497 = ORIENTED_EDGE ( 'NONE', *, *, #9490, .T. ) ;
#16498 = ORIENTED_EDGE ( 'NONE', *, *, #16552, .F. ) ;
#16499 = DIRECTION ( 'NONE',  ( -1.000000000000000000, -0.000000000000000000, -0.000000000000000000 ) ) ;
#16500 = CARTESIAN_POINT ( 'NONE',  ( 53.71875000000000711, 14.00000000000001066, 16.65685424949235482 ) ) ;
#16501 = ORIENTED_EDGE ( 'NONE', *, *, #7350, .F. ) ;
#16502 = ORIENTED_EDGE ( 'NONE', *, *, #10889, .T. ) ;
#16503 = CARTESIAN_POINT ( 'NONE',  ( 51.87731816583844591, 7.123453452023657206, 12.21969229848395599 ) ) ;
#16504 = CARTESIAN_POINT ( 'NONE',  ( 70.80000000109248504, 9.143825827087050939, 12.93301269999999370 ) ) ;
#16505 = CARTESIAN_POINT ( 'NONE',  ( 4.999999999999999112, -6.807171995660630692, 6.478011392632865295 ) ) ;
#16506 = PLANE ( 'NONE',  #11814 ) ;
#16507 = LINE ( 'NONE', #7418, #8754 ) ;
#16508 = ORIENTED_EDGE ( 'NONE', *, *, #846, .F. ) ;
#16509 = CARTESIAN_POINT ( 'NONE',  ( 4.000000000000000888, 4.898587196589412829E-16, 18.62500000273119483 ) ) ;
#16510 =( REPRESENTATION_RELATIONSHIP ('NONE','NONE', #8403, #15757 ) REPRESENTATION_RELATIONSHIP_WITH_TRANSFORMATION ( #22999 )SHAPE_REPRESENTATION_RELATIONSHIP( ) );
#16511 = EDGE_CURVE ( 'NONE', #2967, #15279, #3769, .T. ) ;
#16512 = LINE ( 'NONE', #11016, #357 ) ;
#16513 = EDGE_CURVE ( 'NONE', #23289, #23683, #16854, .T. ) ;
#16514 = CARTESIAN_POINT ( 'NONE',  ( 53.77893183416158251, 8.411196891453236901, 10.97181229448535511 ) ) ;
#16515 = DIRECTION ( 'NONE',  ( 1.224646799147353207E-16, -0.000000000000000000, 1.000000000000000000 ) ) ;
#16516 = CYLINDRICAL_SURFACE ( 'NONE', #4942, 2.500000000000002220 ) ;
#16517 = CARTESIAN_POINT ( 'NONE',  ( -3.019423509283438722, -8.974600000000002353, 10.00000000000008882 ) ) ;
#16518 = CARTESIAN_POINT ( 'NONE',  ( 1.600000000000004086, 9.887492094615969966E-16, 8.073750000000021743 ) ) ;
#16519 = ORIENTED_EDGE ( 'NONE', *, *, #22829, .F. ) ;
#16520 = LINE ( 'NONE', #10911, #9703 ) ;
#16521 = CARTESIAN_POINT ( 'NONE',  ( 53.90625000000000000, 12.99999999999999645, 13.75735931288070191 ) ) ;
#16522 = CARTESIAN_POINT ( 'NONE',  ( 44.00000000000000711, -15.00000000000001954, 10.00000000000008882 ) ) ;
#16523 = FILL_AREA_STYLE ('',( #11382 ) ) ;
#16524 = ADVANCED_FACE ( 'NONE', ( #18620 ), #9306, .T. ) ;
#16525 = VERTEX_POINT ( 'NONE', #2332 ) ;
#16526 = DIRECTION ( 'NONE',  ( 0.000000000000000000, 0.000000000000000000, -1.000000000000000000 ) ) ;
#16527 = LINE ( 'NONE', #18900, #22049 ) ;
#16528 = LINE ( 'NONE', #465, #12106 ) ;
#16529 = ORIENTED_EDGE ( 'NONE', *, *, #9963, .T. ) ;
#16530 = CARTESIAN_POINT ( 'NONE',  ( 3.349226789952652439, 2.685125164760731487, -0.2236248678334773199 ) ) ;
#16531 = ORIENTED_EDGE ( 'NONE', *, *, #23679, .T. ) ;
#16532 = CARTESIAN_POINT ( 'NONE',  ( 19.99999999999998934, 9.999999999999964473, -50.00000000000000000 ) ) ;
#16533 = CARTESIAN_POINT ( 'NONE',  ( 2.828427124746191179, 2.828427124746190291, 17.62500000000001066 ) ) ;
#16534 = DIRECTION ( 'NONE',  ( 1.000000000000000000, 0.000000000000000000, 0.000000000000000000 ) ) ;
#16535 = CARTESIAN_POINT ( 'NONE',  ( 6.500000000000000000, 3.752776749732563477, -3.700000000000000178 ) ) ;
#16536 = DIRECTION ( 'NONE',  ( 0.000000000000000000, 0.000000000000000000, 1.000000000000000000 ) ) ;
#16537 = EDGE_CURVE ( 'NONE', #17065, #10047, #4256, .T. ) ;
#16538 = ORIENTED_EDGE ( 'NONE', *, *, #20866, .F. ) ;
#16539 = EDGE_CURVE ( 'NONE', #13221, #3801, #5692, .T. ) ;
#16540 = CARTESIAN_POINT ( 'NONE',  ( -66.90000000000000568, 9.999999999999998224, 17.49999999999999645 ) ) ;
#16541 = EDGE_CURVE ( 'NONE', #17904, #19658, #9195, .T. ) ;
#16542 = CIRCLE ( 'NONE', #21871, 8.749000000000002331 ) ;
#16543 = CARTESIAN_POINT ( 'NONE',  ( 4.000000000000000000, 4.898587196589412829E-16, -0.07499999726881187434 ) ) ;
#16544 = CARTESIAN_POINT ( 'NONE',  ( 67.55000000109247082, 8.538419263543524096, 13.53841926354352054 ) ) ;
#16545 = CARTESIAN_POINT ( 'NONE',  ( -1.432654583217638944, 3.458734125000000326, 16.25000000136560629 ) ) ;
#16546 = DIRECTION ( 'NONE',  ( -1.000000000000000000, -7.703719777548943412E-32, 0.000000000000000000 ) ) ;
#16547 = CARTESIAN_POINT ( 'NONE',  ( 7.347880794884118750E-16, -4.000000000000000000, 5.550000000000000711 ) ) ;
#16548 = FACE_OUTER_BOUND ( 'NONE', #842, .T. ) ;
#16549 = CARTESIAN_POINT ( 'NONE',  ( 3.458734125000002102, -1.432654583217639610, 12.87500000136560629 ) ) ;
#16550 = DIRECTION ( 'NONE',  ( 0.000000000000000000, 1.224646799147353207E-16, 1.000000000000000000 ) ) ;
#16551 = EDGE_CURVE ( 'NONE', #6074, #6488, #7273, .T. ) ;
#16552 = EDGE_CURVE ( 'NONE', #1359, #8014, #3038, .T. ) ;
#16553 = ORIENTED_EDGE ( 'NONE', *, *, #4864, .F. ) ;
#16554 = CARTESIAN_POINT ( 'NONE',  ( -67.95000000109247651, 11.46158073645647235, 16.46158073645647235 ) ) ;
#16555 = ORIENTED_EDGE ( 'NONE', *, *, #3759, .T. ) ;
#16556 = CARTESIAN_POINT ( 'NONE',  ( 57.15393183416157541, 5.971812294485358663, 16.58880310854675599 ) ) ;
#16557 = CARTESIAN_POINT ( 'NONE',  ( -70.10000000109245377, 7.933012699999995476, 14.14382582708705094 ) ) ;
#16558 = CARTESIAN_POINT ( 'NONE',  ( -2.449293598294706907E-16, 4.000000000000000000, -2.949999999999997957 ) ) ;
#16559 = VERTEX_POINT ( 'NONE', #2444 ) ;
#16560 = ORIENTED_EDGE ( 'NONE', *, *, #22356, .F. ) ;
#16561 = CARTESIAN_POINT ( 'NONE',  ( 3.458734125000001658, 1.432654583217640498, 19.25000000136560274 ) ) ;
#16562 = CARTESIAN_POINT ( 'NONE',  ( 51.03356816583844591, 11.31069182806492712, 17.97181229448534623 ) ) ;
#16563 = CARTESIAN_POINT ( 'NONE',  ( -71.00000000109247367, 12.06698730000000275, 14.14382582708705094 ) ) ;
#16564 = CARTESIAN_POINT ( 'NONE',  ( -70.85000000109246798, 7.933012699999995476, 14.99999999999999645 ) ) ;
#16565 = CARTESIAN_POINT ( 'NONE',  ( 3.458734125000001658, 4.235727675282972223E-16, 13.18750000136560452 ) ) ;
#16566 = EDGE_CURVE ( 'NONE', #13420, #16346, #16446, .T. ) ;
#16567 = CARTESIAN_POINT ( 'NONE',  ( -4.203833317240879275, -1.627343821129593859, -3.597273115243890818 ) ) ;
#16568 = CARTESIAN_POINT ( 'NONE',  ( 60.34143183416158962, 8.689308171935088865, 17.97181229448535689 ) ) ;
#16569 = CARTESIAN_POINT ( 'NONE',  ( -9.000000000000000000, 1.102182119232617714E-15, -3.999999999999999112 ) ) ;
#16570 = EDGE_CURVE ( 'NONE', #17536, #23404, #17220, .T. ) ;
#16571 =( BOUNDED_CURVE ( )  B_SPLINE_CURVE ( 2, ( #20212, #16888, #20691, #2484, #4295, #18429, #5975, #16637, #11632 ),
 .UNSPECIFIED., .F., .F. ) 
 B_SPLINE_CURVE_WITH_KNOTS ( ( 3, 2, 2, 2, 3 ),
 ( 0.4000000000000000222, 0.4124999999999999778, 0.4249999999999999889, 0.4375000000000000000, 0.4500000000000000111 ),
 .UNSPECIFIED. ) 
 CURVE ( )  GEOMETRIC_REPRESENTATION_ITEM ( )  RATIONAL_B_SPLINE_CURVE ( ( 1.000000000000000000, 0.9238795325112867385, 1.000000000000000000, 0.9238795325112867385, 1.000000000000000000, 0.9238795325112867385, 1.000000000000000000, 0.9238795325112867385, 1.000000000000000000 ) ) 
 REPRESENTATION_ITEM ( '' )  );
#16572 = CARTESIAN_POINT ( 'NONE',  ( 53.81250000000000711, 13.00000000000000000, 14.99999999999998757 ) ) ;
#16573 = CARTESIAN_POINT ( 'NONE',  ( 1.656854249492384135, -3.999999999999999112, 17.43750000273119483 ) ) ;
#16574 = DIRECTION ( 'NONE',  ( 1.000000000000000000, 0.000000000000000000, 0.000000000000000000 ) ) ;
#16575 = EDGE_CURVE ( 'NONE', #18117, #3012, #4679, .T. ) ;
#16576 = VECTOR ( 'NONE', #17444, 1000.000000000000000 ) ;
#16577 = EDGE_LOOP ( 'NONE', ( #577, #18704, #10276 ) ) ;
#16578 = DIRECTION ( 'NONE',  ( 1.000000000000000000, 0.000000000000000000, 0.000000000000000000 ) ) ;
#16579 = ORIENTED_EDGE ( 'NONE', *, *, #4274, .F. ) ;
#16580 = CARTESIAN_POINT ( 'NONE',  ( 51.46875000000000000, 6.999999999999992895, 13.75735931288071967 ) ) ;
#16581 =( NAMED_UNIT ( * ) SI_UNIT ( $, .STERADIAN. ) SOLID_ANGLE_UNIT ( ) );
#16582 = CARTESIAN_POINT ( 'NONE',  ( 3.458734125000000326, 1.432654583217640498, 4.300000001365595459 ) ) ;
#16583 = CARTESIAN_POINT ( 'NONE',  ( -4.350941807883110357, -4.993536075455427437, -0.06682554136338243744 ) ) ;
#16584 = ORIENTED_EDGE ( 'NONE', *, *, #13815, .T. ) ;
#16585 = CARTESIAN_POINT ( 'NONE',  ( 2.828427124746191179, 2.828427124746190291, 18.62500000000001066 ) ) ;
#16586 = CYLINDRICAL_SURFACE ( 'NONE', #2222, 11.00000000000000000 ) ;
#16587 = AXIS2_PLACEMENT_3D ( 'NONE', #23105, #7076, #12609 ) ;
#16588 = CARTESIAN_POINT ( 'NONE',  ( 68.95000000000000284, 11.03553390593269157, 12.49999999999994849 ) ) ;
#16589 = ORIENTED_EDGE ( 'NONE', *, *, #17224, .F. ) ;
#16590 =( NAMED_UNIT ( * ) PLANE_ANGLE_UNIT ( ) SI_UNIT ( $, .RADIAN. ) );
#16591 = PRODUCT_DEFINITION_SHAPE ( 'NONE', 'NONE',  #23702 ) ;
#16592 = CARTESIAN_POINT ( 'NONE',  ( -35.00000000000000000, 4.500000000000001776, -19.99999999999998934 ) ) ;
#16593 = CARTESIAN_POINT ( 'NONE',  ( 6.353591512924457348E-16, -3.458734125000000770, -0.7624999986344024316 ) ) ;
#16594 = CIRCLE ( 'NONE', #18877, 11.00000000000000000 ) ;
#16595 = CARTESIAN_POINT ( 'NONE',  ( 68.45000000000000284, 11.03553390593273598, 17.50000000000000355 ) ) ;
#16596 = CARTESIAN_POINT ( 'NONE',  ( 50.00000000000000000, -15.00000000000001954, 10.00000000000008882 ) ) ;
#16597 = LINE ( 'NONE', #4010, #3424 ) ;
#16598 = CARTESIAN_POINT ( 'NONE',  ( 51.59606816583843170, 11.58880310854672935, 10.97181229448534445 ) ) ;
#16599 = CARTESIAN_POINT ( 'NONE',  ( 2.445694354108820523, -2.445694354108820079, 1.112500001365595681 ) ) ;
#16600 = CARTESIAN_POINT ( 'NONE',  ( -2.445694354108819191, 2.445694354108820523, 13.56250000136560629 ) ) ;
#16601 = EDGE_CURVE ( 'NONE', #19016, #12637, #11224, .T. ) ;
#16602 = CARTESIAN_POINT ( 'NONE',  ( -71.84999999999999432, 7.499999999999996447, 16.03553390593273775 ) ) ;
#16603 = LINE ( 'NONE', #12567, #3634 ) ;
#16604 = CARTESIAN_POINT ( 'NONE',  ( -3.999999999999999112, 1.656854249492380582, 16.93750000000001066 ) ) ;
#16605 = ORIENTED_EDGE ( 'NONE', *, *, #19420, .F. ) ;
#16606 = DIRECTION ( 'NONE',  ( -3.697785493223484080E-32, -0.3420201433256691015, -0.9396926207859082059 ) ) ;
#16607 = LINE ( 'NONE', #20055, #11786 ) ;
#16608 = CARTESIAN_POINT ( 'NONE',  ( 22.11331769071655984, -8.974600000000002353, 5.000000000000079936 ) ) ;
#16609 = ORIENTED_EDGE ( 'NONE', *, *, #1544, .T. ) ;
#16610 = ORIENTED_EDGE ( 'NONE', *, *, #20166, .T. ) ;
#16611 = CARTESIAN_POINT ( 'NONE',  ( 4.999999999999999112, -10.90201369670497478, -1.464956435139656898 ) ) ;
#16612 = VECTOR ( 'NONE', #23017, 1000.000000000000000 ) ;
#16613 = CARTESIAN_POINT ( 'NONE',  ( 57.65625000000001421, 6.000000000000004441, 16.65685424949239390 ) ) ;
#16614 = EDGE_LOOP ( 'NONE', ( #22336, #19785, #8252, #13884 ) ) ;
#16615 = LINE ( 'NONE', #18286, #11839 ) ;
#16616 = ORIENTED_EDGE ( 'NONE', *, *, #13888, .F. ) ;
#16617 = CARTESIAN_POINT ( 'NONE',  ( 56.37731816583843170, 7.123453452023657206, 12.21969229848395599 ) ) ;
#16618 = AXIS2_PLACEMENT_3D ( 'NONE', #7314, #2242, #21881 ) ;
#16619 = CARTESIAN_POINT ( 'NONE',  ( 66.30000000218494449, 8.232233047033627571, 16.76776695296636532 ) ) ;
#16620 = VECTOR ( 'NONE', #20771, 1000.000000000000000 ) ;
#16621 = CARTESIAN_POINT ( 'NONE',  ( 1.971781867644420635E-15, -4.000000000000000000, 19.25000000000001066 ) ) ;
#16622 = CARTESIAN_POINT ( 'NONE',  ( 70.80000000109245661, 7.933012699999995476, 15.85617417291294196 ) ) ;
#16623 = ORIENTED_EDGE ( 'NONE', *, *, #9134, .T. ) ;
#16624 = CARTESIAN_POINT ( 'NONE',  ( -3.999999999999999112, 1.656854249492380804, 19.06250000273119483 ) ) ;
#16625 = DIRECTION ( 'NONE',  ( 0.000000000000000000, 0.000000000000000000, 1.000000000000000000 ) ) ;
#16626 = CARTESIAN_POINT ( 'NONE',  ( 54.06018183416157541, 5.999999999999996447, 14.93194885905437808 ) ) ;
#16627 = DIRECTION ( 'NONE',  ( -1.000000000000000000, -7.703719777548943412E-32, 0.000000000000000000 ) ) ;
#16628 = CARTESIAN_POINT ( 'NONE',  ( 69.80000000218494449, 9.999999999999998224, 12.49999999999999289 ) ) ;
#16629 = CARTESIAN_POINT ( 'NONE',  ( 72.45000000000001705, 11.03553390593273953, 17.50000000000000355 ) ) ;
#16630 = CARTESIAN_POINT ( 'NONE',  ( 4.000000000000000000, -1.700175430507292473, -3.320327275037661785 ) ) ;
#16631 = ORIENTED_EDGE ( 'NONE', *, *, #3538, .T. ) ;
#16632 = CARTESIAN_POINT ( 'NONE',  ( -3.250000000000003997, -5.629165124598848102, 1.734723475976807094E-15 ) ) ;
#16633 = CARTESIAN_POINT ( 'NONE',  ( -4.197477534772231955, 0.8522413273724368521, -3.505042416683225692 ) ) ;
#16634 = CARTESIAN_POINT ( 'NONE',  ( -90.00000000000000000, 1.012170579495290078E-15, 8.265000000000021885 ) ) ;
#16635 = ORIENTED_EDGE ( 'NONE', *, *, #3894, .F. ) ;
#16636 = FACE_OUTER_BOUND ( 'NONE', #2606, .T. ) ;
#16637 = CARTESIAN_POINT ( 'NONE',  ( 4.000000000000000888, 1.656854249492381248, 14.68750000273119660 ) ) ;
#16638 = CYLINDRICAL_SURFACE ( 'NONE', #9331, 6.000000000000021316 ) ;
#16639 = VECTOR ( 'NONE', #4054, 999.9999999999997726 ) ;
#16640 = SHAPE_REPRESENTATION ( 'spur gear_iso_ISO - Spur gear 1M 20T 20PA 5FW ---S20B12H25L8.0S1', ( #7318 ), #23252 ) ;
#16641 = AXIS2_PLACEMENT_3D ( 'NONE', #13322, #362, #17137 ) ;
#16642 = EDGE_LOOP ( 'NONE', ( #13813, #15659, #18815, #15209 ) ) ;
#16643 = DIRECTION ( 'NONE',  ( -1.000000000000000000, 0.000000000000000000, 0.000000000000000000 ) ) ;
#16644 = ORIENTED_EDGE ( 'NONE', *, *, #9816, .T. ) ;
#16645 = ADVANCED_FACE ( 'NONE', ( #16713 ), #10144, .T. ) ;
#16646 = LINE ( 'NONE', #224, #297 ) ;
#16647 = CARTESIAN_POINT ( 'NONE',  ( 2.828427124746192067, -2.828427124746189847, 16.37500000000001066 ) ) ;
#16648 = DIRECTION ( 'NONE',  ( 0.000000000000000000, 0.000000000000000000, -1.000000000000000000 ) ) ;
#16649 = FACE_OUTER_BOUND ( 'NONE', #4595, .T. ) ;
#16650 = CARTESIAN_POINT ( 'NONE',  ( 66.60000000218495586, 9.999999999999998224, 12.49999999999999289 ) ) ;
#16651 = CARTESIAN_POINT ( 'NONE',  ( 70.00000000109247367, 7.933012699999995476, 15.85617417291294196 ) ) ;
#16652 = EDGE_CURVE ( 'NONE', #13240, #4980, #10387, .T. ) ;
#16653 = ORIENTED_EDGE ( 'NONE', *, *, #17584, .F. ) ;
#16654 = AXIS2_PLACEMENT_3D ( 'NONE', #497, #16920, #2160 ) ;
#16655 = CARTESIAN_POINT ( 'NONE',  ( -68.59999999999999432, 8.232233047033627571, 16.76776695296636532 ) ) ;
#16656 = AXIS2_PLACEMENT_3D ( 'NONE', #8250, #17699, #22958 ) ;
#16657 = CARTESIAN_POINT ( 'NONE',  ( -4.000000000000000000, -1.656854249492383024, -0.5124999972688124572 ) ) ;
#16658 = CARTESIAN_POINT ( 'NONE',  ( 67.45000000109246230, 7.933012699999995476, 14.99999999999999645 ) ) ;
#16659 = CARTESIAN_POINT ( 'NONE',  ( 2.445694354108821855, -2.445694354108820079, 15.81250000136560629 ) ) ;
#16660 = DIRECTION ( 'NONE',  ( 0.000000000000000000, 0.000000000000000000, 1.000000000000000000 ) ) ;
#16661 = CARTESIAN_POINT ( 'NONE',  ( 6.353591512924457348E-16, -3.458734125000000770, -2.762499998634404097 ) ) ;
#16662 = CARTESIAN_POINT ( 'NONE',  ( -1.656854249492380804, 4.000000000000000000, 5.112500000000002487 ) ) ;
#16663 = CARTESIAN_POINT ( 'NONE',  ( -27.50000000000000711, 7.500000000000002665, -31.01025403784447576 ) ) ;
#16664 = CARTESIAN_POINT ( 'NONE',  ( -3.458734124999998993, 0.000000000000000000, 14.43750000136560452 ) ) ;
#16665 = CARTESIAN_POINT ( 'NONE',  ( -67.10000000218495586, 8.232233047033627571, 16.76776695296636532 ) ) ;
#16666 = VECTOR ( 'NONE', #15100, 1000.000000000000000 ) ;
#16667 = EDGE_LOOP ( 'NONE', ( #5211, #20699 ) ) ;
#16668 = CARTESIAN_POINT ( 'NONE',  ( -70.05000000109247082, 9.999999999999998224, 12.93301269999999192 ) ) ;
#16669 = ORIENTED_EDGE ( 'NONE', *, *, #4603, .T. ) ;
#16670 = CARTESIAN_POINT ( 'NONE',  ( 58.18518183416157541, 10.06805114094561659, 10.99999999999999645 ) ) ;
#16671 = CARTESIAN_POINT ( 'NONE',  ( -70.20000000109246230, 9.143825827087050939, 12.93301269999999370 ) ) ;
#16672 = APPLICATION_PROTOCOL_DEFINITION ( 'draft international standard', 'automotive_design', 1998, #1495 ) ;
#16673 = DIRECTION ( 'NONE',  ( -0.3420201433256622181, 0.9396926207859106484, 1.232595164407828100E-31 ) ) ;
#16674 = VERTEX_POINT ( 'NONE', #1002 ) ;
#16675 = EDGE_CURVE ( 'NONE', #17274, #14810, #12815, .T. ) ;
#16676 = AXIS2_PLACEMENT_3D ( 'NONE', #23356, #14158, #17738 ) ;
#16677 = EDGE_CURVE ( 'NONE', #15450, #6430, #15419, .T. ) ;
#16678 = EDGE_LOOP ( 'NONE', ( #18905, #2667 ) ) ;
#16679 = AXIS2_PLACEMENT_3D ( 'NONE', #13146, #20409, #16491 ) ;
#16680 = CARTESIAN_POINT ( 'NONE',  ( 2.445694354108822299, -2.445694354108820079, 16.06250000136560629 ) ) ;
#16681 = CARTESIAN_POINT ( 'NONE',  ( 53.53125000000000000, 11.24264068711929276, 18.00000000000000355 ) ) ;
#16682 = CARTESIAN_POINT ( 'NONE',  ( -70.70000000109247651, 7.933012699999995476, 14.14382582708705094 ) ) ;
#16683 = EDGE_CURVE ( 'NONE', #22841, #3346, #6883, .T. ) ;
#16684 = ADVANCED_FACE ( 'NONE', ( #8218 ), #13854, .F. ) ;
#16685 = CARTESIAN_POINT ( 'NONE',  ( -70.50000000109245946, 12.06698730000000275, 15.85617417291294196 ) ) ;
#16686 = CARTESIAN_POINT ( 'NONE',  ( -2.445694354108819191, 2.445694354108820523, 10.56250000136560629 ) ) ;
#16687 = CARTESIAN_POINT ( 'NONE',  ( -60.00000000000000711, 9.999999999999998224, 14.99999999999999645 ) ) ;
#16688 = CARTESIAN_POINT ( 'NONE',  ( 60.06018183416157541, 7.000000000000000000, 14.93194885905437097 ) ) ;
#16689 = CARTESIAN_POINT ( 'NONE',  ( -20.00000000000001066, 9.999999999999964473, -49.99999999999999289 ) ) ;
#16690 = CARTESIAN_POINT ( 'NONE',  ( 1.432654583217643163, -3.458734124999999437, 11.75000000136560629 ) ) ;
#16691 = CARTESIAN_POINT ( 'NONE',  ( 4.000000000000000888, 1.656854249492381248, 17.68750000273119483 ) ) ;
#16692 = CARTESIAN_POINT ( 'NONE',  ( 68.79999999999999716, 8.232233047033629347, 13.23223304703362402 ) ) ;
#16693 = VERTEX_POINT ( 'NONE', #21225 ) ;
#16694 = CARTESIAN_POINT ( 'NONE',  ( 70.29999999999999716, 7.499999999999996447, 14.99999999999999645 ) ) ;
#16695 = CARTESIAN_POINT ( 'NONE',  ( -70.39999999999999147, 8.232233047033629347, 13.23223304703362402 ) ) ;
#16696 = ORIENTED_EDGE ( 'NONE', *, *, #5686, .T. ) ;
#16697 = CARTESIAN_POINT ( 'NONE',  ( 57.18750000000000000, 9.999999999999989342, 11.99999999999999467 ) ) ;
#16698 = CARTESIAN_POINT ( 'NONE',  ( -3.458734125000000326, 0.000000000000000000, 4.737500001365595459 ) ) ;
#16699 = ADVANCED_FACE ( 'NONE', ( #18973 ), #15535, .T. ) ;
#16700 = FACE_OUTER_BOUND ( 'NONE', #6186, .T. ) ;
#16701 = ORIENTED_EDGE ( 'NONE', *, *, #22400, .T. ) ;
#16702 = CARTESIAN_POINT ( 'NONE',  ( -1.656854249492380138, -3.999999999999999112, 15.18750000000001066 ) ) ;
#16703 = CARTESIAN_POINT ( 'NONE',  ( -10.00000000000000000, 0.000000000000000000, 0.000000000000000000 ) ) ;
#16704 = EDGE_CURVE ( 'NONE', #3848, #17653, #10030, .T. ) ;
#16705 = CARTESIAN_POINT ( 'NONE',  ( 4.999999999999999112, -9.314797388894900720, 5.239665997526855357 ) ) ;
#16706 = ORIENTED_EDGE ( 'NONE', *, *, #20670, .F. ) ;
#16707 = CYLINDRICAL_SURFACE ( 'NONE', #18618, 4.000000000000001776 ) ;
#16708 = EDGE_CURVE ( 'NONE', #17879, #8889, #10293, .T. ) ;
#16709 = CARTESIAN_POINT ( 'NONE',  ( -3.458734125000000326, -0.5784715375562745621, 2.012736001390157181 ) ) ;
#16710 = EDGE_CURVE ( 'NONE', #9090, #23518, #17553, .T. ) ;
#16711 = CARTESIAN_POINT ( 'NONE',  ( 69.89999999999999147, 12.50000000000000000, 14.99999999999999645 ) ) ;
#16712 = CARTESIAN_POINT ( 'NONE',  ( 45.00000000000000000, -2.399706452296378245, 55.00000000000021316 ) ) ;
#16713 = FACE_OUTER_BOUND ( 'NONE', #21508, .T. ) ;
#16714 = CARTESIAN_POINT ( 'NONE',  ( 52.72106816583844591, 14.02818770551465377, 16.58880310854672757 ) ) ;
#16715 = CARTESIAN_POINT ( 'NONE',  ( 2.445694354108820079, 2.445694354108820523, 0.3625000013655951259 ) ) ;
#16716 = CARTESIAN_POINT ( 'NONE',  ( 1.025207404391860050E-15, 3.458734125000000770, 13.43750000136560452 ) ) ;
#16717 = DIRECTION ( 'NONE',  ( 1.000000000000000000, -0.000000000000000000, -0.000000000000000000 ) ) ;
#16718 = DIRECTION ( 'NONE',  ( 0.000000000000000000, -0.000000000000000000, -1.000000000000000000 ) ) ;
#16719 = VECTOR ( 'NONE', #17859, 1000.000000000000000 ) ;
#16720 = CARTESIAN_POINT ( 'NONE',  ( 4.999999999999999112, -3.174628368996021521, -8.152713396088794084 ) ) ;
#16721 = ORIENTED_EDGE ( 'NONE', *, *, #19183, .F. ) ;
#16722 = CARTESIAN_POINT ( 'NONE',  ( -1.656854249492379472, 4.000000000000000000, 11.93750000273119660 ) ) ;
#16723 = CARTESIAN_POINT ( 'NONE',  ( 0.000000000000000000, 0.000000000000000000, 0.000000000000000000 ) ) ;
#16724 = LINE ( 'NONE', #303, #19629 ) ;
#16725 = ORIENTED_EDGE ( 'NONE', *, *, #15671, .T. ) ;
#16726 = VERTEX_POINT ( 'NONE', #19324 ) ;
#16727 = AXIS2_PLACEMENT_3D ( 'NONE', #1585, #10734, #20223 ) ;
#16728 = LINE ( 'NONE', #22215, #7562 ) ;
#16729 = CARTESIAN_POINT ( 'NONE',  ( 54.46875000000000000, 5.999999999999987566, 13.34314575050763452 ) ) ;
#16730 = ORIENTED_EDGE ( 'NONE', *, *, #9423, .T. ) ;
#16731 = DIRECTION ( 'NONE',  ( 0.06805114094563399774, -0.7054675904022866817, -0.7054675904022729149 ) ) ;
#16732 = ORIENTED_EDGE ( 'NONE', *, *, #547, .F. ) ;
#16733 = CIRCLE ( 'NONE', #14855, 4.000000000000001776 ) ;
#16734 = VECTOR ( 'NONE', #1580, 1000.000000000000000 ) ;
#16735 = CARTESIAN_POINT ( 'NONE',  ( 52.06481816583844591, 5.999999999999996447, 15.06805114094564502 ) ) ;
#16736 = ADVANCED_FACE ( 'NONE', ( #23481 ), #884, .T. ) ;
#16737 = CARTESIAN_POINT ( 'NONE',  ( 71.40000000109249356, 7.933012699999995476, 15.85617417291294196 ) ) ;
#16738 = EDGE_CURVE ( 'NONE', #23245, #23109, #20994, .T. ) ;
#16739 = AXIS2_PLACEMENT_3D ( 'NONE', #16338, #3153, #7247 ) ;
#16740 = CARTESIAN_POINT ( 'NONE',  ( 71.60000000109246798, 7.933012699999995476, 15.85617417291294196 ) ) ;
#16741 = EDGE_LOOP ( 'NONE', ( #18756, #3602, #21771, #4886 ) ) ;
#16742 = CARTESIAN_POINT ( 'NONE',  ( 9.920644283265380691E-16, 4.000000000000000000, 18.87500000273119838 ) ) ;
#16743 = AXIS2_PLACEMENT_3D ( 'NONE', #10790, #16163, #5017 ) ;
#16744 = CARTESIAN_POINT ( 'NONE',  ( -4.000000000000000888, 1.656854249492380582, 0.3625000027311864881 ) ) ;
#16745 = CARTESIAN_POINT ( 'NONE',  ( 53.87268183416157541, 7.219692298483935566, 12.12345345202367675 ) ) ;
#16746 = CARTESIAN_POINT ( 'NONE',  ( -19.99999999999999645, -9.000000000000003553, 10.00000000000008882 ) ) ;
#16747 = LINE ( 'NONE', #328, #2068 ) ;
#16748 = CIRCLE ( 'NONE', #20928, 12.00000000000000000 ) ;
#16749 = CARTESIAN_POINT ( 'NONE',  ( -2.762848947613220307, 4.746226468750993632, -26.84672628368516811 ) ) ;
#16750 = VECTOR ( 'NONE', #900, 1000.000000000000000 ) ;
#16751 = LINE ( 'NONE', #16992, #15147 ) ;
#16752 = CARTESIAN_POINT ( 'NONE',  ( 5.968343123267133343, -4.059728990630809164, -3.296662375310746906 ) ) ;
#16753 = VERTEX_POINT ( 'NONE', #11705 ) ;
#16754 = LINE ( 'NONE', #21117, #16576 ) ;
#16755 = CARTESIAN_POINT ( 'NONE',  ( 53.81250000000000711, 13.00000000000000000, 14.99999999999998757 ) ) ;
#16756 = DIRECTION ( 'NONE',  ( 0.000000000000000000, 0.000000000000000000, 1.000000000000000000 ) ) ;
#16757 =( NAMED_UNIT ( * ) SI_UNIT ( $, .STERADIAN. ) SOLID_ANGLE_UNIT ( ) );
#16758 = ORIENTED_EDGE ( 'NONE', *, *, #6897, .F. ) ;
#16759 = CARTESIAN_POINT ( 'NONE',  ( 0.000000000000000000, 8.475820894092974456, 4.057423117305423155 ) ) ;
#16760 = CARTESIAN_POINT ( 'NONE',  ( 70.75000000000000000, 12.50000000000000000, 16.03553390593273775 ) ) ;
#16761 = CARTESIAN_POINT ( 'NONE',  ( 22.71892870323381075, -9.000000000000005329, 5.000000000000079936 ) ) ;
#16762 = CARTESIAN_POINT ( 'NONE',  ( 1.971781867644420635E-15, -4.000000000000000000, 16.37500000273119838 ) ) ;
#16763 = VERTEX_POINT ( 'NONE', #4614 ) ;
#16764 = CARTESIAN_POINT ( 'NONE',  ( -20.00000000000001066, 4.500000000000003553, -50.00000000000000000 ) ) ;
#16765 = ORIENTED_EDGE ( 'NONE', *, *, #1108, .T. ) ;
#16766 = AXIS2_PLACEMENT_3D ( 'NONE', #5863, #17006, #581 ) ;
#16767 = CARTESIAN_POINT ( 'NONE',  ( 2.059999999999998721, 0.000000000000000000, -0.3080913168122742518 ) ) ;
#16768 = CARTESIAN_POINT ( 'NONE',  ( -1.656854249492380138, -3.999999999999999112, 14.18750000000001066 ) ) ;
#16769 = CARTESIAN_POINT ( 'NONE',  ( -3.999999999999999112, 0.000000000000000000, 21.31370849898476649 ) ) ;
#16770 = AXIS2_PLACEMENT_3D ( 'NONE', #13870, #21128, #15784 ) ;
#16771 = AXIS2_PLACEMENT_3D ( 'NONE', #21844, #4000, #11459 ) ;
#16772 = DIRECTION ( 'NONE',  ( -0.000000000000000000, 0.000000000000000000, -1.000000000000000000 ) ) ;
#16773 =( GEOMETRIC_REPRESENTATION_CONTEXT ( 3 ) GLOBAL_UNCERTAINTY_ASSIGNED_CONTEXT ( ( #16975 ) ) GLOBAL_UNIT_ASSIGNED_CONTEXT ( ( #15045, #15401, #3015 ) ) REPRESENTATION_CONTEXT ( 'NONE', 'WORKASPACE' ) );
#16774 = DIRECTION ( 'NONE',  ( 0.3420201433256622181, 0.9396926207859107594, -6.162975822039141593E-32 ) ) ;
#16775 = CARTESIAN_POINT ( 'NONE',  ( 72.20000000109246230, 10.85617417291294551, 17.06698730000000097 ) ) ;
#16776 = ORIENTED_EDGE ( 'NONE', *, *, #16015, .F. ) ;
#16777 = DIRECTION ( 'NONE',  ( -1.000000000000000000, -0.000000000000000000, -0.000000000000000000 ) ) ;
#16778 = DIRECTION ( 'NONE',  ( -1.000000000000000000, 0.000000000000000000, 0.000000000000000000 ) ) ;
#16779 = CARTESIAN_POINT ( 'NONE',  ( 66.25000000109247367, 12.06698730000000097, 14.99999999999999645 ) ) ;
#16780 = CARTESIAN_POINT ( 'NONE',  ( -1.432654583217638944, 3.458734125000000326, 17.25000000136560274 ) ) ;
#16781 = CARTESIAN_POINT ( 'NONE',  ( 4.197393957002303999, -0.4069871074557456780, -3.503767560748925813 ) ) ;
#16782 = EDGE_CURVE ( 'NONE', #2702, #14967, #2556, .T. ) ;
#16783 = PLANE ( 'NONE',  #23362 ) ;
#16784 = CARTESIAN_POINT ( 'NONE',  ( -4.000000000000000000, 0.000000000000000000, 1.300000000000000711 ) ) ;
#16785 = CARTESIAN_POINT ( 'NONE',  ( 2.828427124746191179, 2.828427124746190291, 12.62500000000001066 ) ) ;
#16786 = CARTESIAN_POINT ( 'NONE',  ( 2.445694354108821411, 2.445694354108820523, 13.06250000136560452 ) ) ;
#16787 = FACE_OUTER_BOUND ( 'NONE', #21953, .T. ) ;
#16788 = PRODUCT_DEFINITION_SHAPE ( 'NONE', 'NONE',  #23712 ) ;
#16789 = VERTEX_POINT ( 'NONE', #17199 ) ;
#16790 = CARTESIAN_POINT ( 'NONE',  ( -69.95000000109247651, 8.538419263543524096, 13.53841926354352054 ) ) ;
#16791 = ORIENTED_EDGE ( 'NONE', *, *, #4663, .F. ) ;
#16792 = CARTESIAN_POINT ( 'NONE',  ( 59.62500000000000711, 12.82842712474620228, 17.82842712474617386 ) ) ;
#16793 = CARTESIAN_POINT ( 'NONE',  ( -65.70000000109249072, 9.143825827087049163, 17.06698729999999742 ) ) ;
#16794 = PRODUCT_CONTEXT ( 'NONE', #17102, 'mechanical' ) ;
#16795 = AXIS2_PLACEMENT_3D ( 'NONE', #19491, #1165, #2841 ) ;
#16796 = VERTEX_POINT ( 'NONE', #11948 ) ;
#16797 = PLANE ( 'NONE',  #14784 ) ;
#16798 = ORIENTED_EDGE ( 'NONE', *, *, #10206, .T. ) ;
#16799 = EDGE_LOOP ( 'NONE', ( #6868, #5797, #23494, #16730 ) ) ;
#16800 = CARTESIAN_POINT ( 'NONE',  ( 1.025207404391860050E-15, 3.458734125000000770, 15.43750000136560452 ) ) ;
#16801 = AXIS2_PLACEMENT_3D ( 'NONE', #1058, #2389, #13318 ) ;
#16802 = CARTESIAN_POINT ( 'NONE',  ( 53.62500000000000711, 12.12132034355964727, 17.12132034355963484 ) ) ;
#16803 = VECTOR ( 'NONE', #21762, 1000.000000000000000 ) ;
#16804 = CARTESIAN_POINT ( 'NONE',  ( -67.25000000109247367, 9.999999999999998224, 17.06698730000000097 ) ) ;
#16805 = CARTESIAN_POINT ( 'NONE',  ( 68.20000000109246230, 7.933012699999995476, 15.85617417291294196 ) ) ;
#16806 = CARTESIAN_POINT ( 'NONE',  ( -0.9709838737629333805, 3.325368937167130223, -3.295601554149325541 ) ) ;
#16807 = CARTESIAN_POINT ( 'NONE',  ( -67.20000000109247651, 12.06698730000000275, 14.14382582708705094 ) ) ;
#16808 = TOROIDAL_SURFACE ( 'NONE', #15312, 6.760799999999997034, 0.03079999999999857851 ) ;
#16809 = CARTESIAN_POINT ( 'NONE',  ( 2.445694354108821411, 2.445694354108820523, 13.31250000136560452 ) ) ;
#16810 = DIRECTION ( 'NONE',  ( 0.3420201433256622181, 0.9396926207859107594, -6.162975822039141593E-32 ) ) ;
#16811 = CARTESIAN_POINT ( 'NONE',  ( 56.02893183416158962, 11.17458954617365663, 18.02818770551464311 ) ) ;
#16812 = LINE ( 'NONE', #7831, #2787 ) ;
#16813 = ADVANCED_FACE ( 'NONE', ( #3039 ), #16316, .F. ) ;
#16814 = CARTESIAN_POINT ( 'NONE',  ( 52.59375000000000711, 11.24264068711927322, 11.99999999999998934 ) ) ;
#16815 = EDGE_CURVE ( 'NONE', #9313, #17013, #13434, .T. ) ;
#16816 = CARTESIAN_POINT ( 'NONE',  ( 1.567478505476135000E-15, 4.618802153517012954, -3.504269196027527844 ) ) ;
#16817 = CARTESIAN_POINT ( 'NONE',  ( 2.828427124746191179, 2.828427124746190291, 17.75000000273119483 ) ) ;
#16818 = VECTOR ( 'NONE', #8156, 1000.000000000000000 ) ;
#16819 = CARTESIAN_POINT ( 'NONE',  ( 50.00000000000000000, 18.33638201715224270, 11.21434374438452508 ) ) ;
#16820 = VECTOR ( 'NONE', #7855, 1000.000000000000000 ) ;
#16821 = VERTEX_POINT ( 'NONE', #11177 ) ;
#16822 = DIRECTION ( 'NONE',  ( 0.000000000000000000, 0.000000000000000000, -1.000000000000000000 ) ) ;
#16823 = CARTESIAN_POINT ( 'NONE',  ( 0.1410422978106145031, -4.700232962125109104, -3.687027686973628704 ) ) ;
#16824 = ORIENTED_EDGE ( 'NONE', *, *, #14217, .T. ) ;
#16825 = CARTESIAN_POINT ( 'NONE',  ( 56.59143183416158962, 11.31069182806491291, 12.02818770551463778 ) ) ;
#16826 = CARTESIAN_POINT ( 'NONE',  ( 1.656854249492383024, -3.999999999999999112, -2.262499997268812013 ) ) ;
#16827 = EDGE_CURVE ( 'NONE', #315, #9317, #7095, .T. ) ;
#16828 = CARTESIAN_POINT ( 'NONE',  ( -4.623144047065557594, -4.836380039389424290, -0.1061556211655376447 ) ) ;
#16829 = ORIENTED_EDGE ( 'NONE', *, *, #6906, .F. ) ;
#16830 = CARTESIAN_POINT ( 'NONE',  ( -2.828427124746188515, -2.828427124746190735, 13.12500000000001243 ) ) ;
#16831 = FACE_OUTER_BOUND ( 'NONE', #17121, .T. ) ;
#16832 = PRESENTATION_LAYER_ASSIGNMENT (  '', '', ( #2279 ) ) ;
#16833 = ORIENTED_EDGE ( 'NONE', *, *, #19880, .F. ) ;
#16834 = CARTESIAN_POINT ( 'NONE',  ( -71.50000000218496155, 11.76776695296636888, 13.23223304703362579 ) ) ;
#16835 = CARTESIAN_POINT ( 'NONE',  ( 3.458734125000000770, 4.235727675282972223E-16, 1.487500001365596125 ) ) ;
#16836 = AXIS2_PLACEMENT_3D ( 'NONE', #7054, #14374, #1644 ) ;
#16837 = AXIS2_PLACEMENT_3D ( 'NONE', #6562, #21136, #4749 ) ;
#16838 = CARTESIAN_POINT ( 'NONE',  ( 66.94999999999998863, 8.964466094067258695, 17.50000000000000355 ) ) ;
#16839 = DIRECTION ( 'NONE',  ( -0.000000000000000000, -1.000000000000000000, -0.000000000000000000 ) ) ;
#16840 = VECTOR ( 'NONE', #19357, 1000.000000000000000 ) ;
#16841 = CARTESIAN_POINT ( 'NONE',  ( 1.734723475976807094E-15, 4.618802153517012954, -0.4999999999999995559 ) ) ;
#16842 = VECTOR ( 'NONE', #2060, 1000.000000000000000 ) ;
#16843 = CARTESIAN_POINT ( 'NONE',  ( 54.12731816583844591, 12.87654654797634102, 17.78030770151602979 ) ) ;
#16844 = ADVANCED_FACE ( 'NONE', ( #9369 ), #7344, .T. ) ;
#16845 = CARTESIAN_POINT ( 'NONE',  ( 3.458734125000000770, 1.432654583217640498, 4.550000001365596347 ) ) ;
#16846 = CARTESIAN_POINT ( 'NONE',  ( 2.445694354108822299, -2.445694354108820079, 14.06250000136560629 ) ) ;
#16847 = DIRECTION ( 'NONE',  ( -0.9396926207859107594, -0.3420201433256623291, 1.540743955509804830E-32 ) ) ;
#16848 = CARTESIAN_POINT ( 'NONE',  ( -71.95000000109247651, 11.46158073645647235, 13.53841926354352232 ) ) ;
#16849 = DIRECTION ( 'NONE',  ( 1.000000000000000000, 0.000000000000000000, 0.000000000000000000 ) ) ;
#16850 = ORIENTED_EDGE ( 'NONE', *, *, #15671, .F. ) ;
#16851 = CARTESIAN_POINT ( 'NONE',  ( 9.920644283265380691E-16, 4.000000000000000000, 11.87500000273119660 ) ) ;
#16852 = DIRECTION ( 'NONE',  ( -1.000000000000000000, 0.000000000000000000, 0.000000000000000000 ) ) ;
#16853 = CARTESIAN_POINT ( 'NONE',  ( -71.65000000109247935, 9.999999999999998224, 12.93301269999999192 ) ) ;
#16854 = B_SPLINE_CURVE_WITH_KNOTS ( 'NONE', 3,
 ( #17074, #648, #176, #11348, #13139, #16841 ),
 .UNSPECIFIED., .F., .F.,
 ( 4, 2, 4 ),
 ( 0.002365888236227977302, 0.003551327329835078910, 0.004736766423442180518 ),
 .UNSPECIFIED. ) ;
#16855 = EDGE_CURVE ( 'NONE', #20420, #15433, #22947, .T. ) ;
#16856 = ORIENTED_EDGE ( 'NONE', *, *, #4392, .F. ) ;
#16857 = EDGE_CURVE ( 'NONE', #19235, #20146, #8439, .T. ) ;
#16858 = ORIENTED_EDGE ( 'NONE', *, *, #5092, .F. ) ;
#16859 = DIRECTION ( 'NONE',  ( 1.000000000000000000, 0.000000000000000000, 0.000000000000000000 ) ) ;
#16860 = DIRECTION ( 'NONE',  ( -0.000000000000000000, -0.000000000000000000, 1.000000000000000000 ) ) ;
#16861 = ORIENTED_EDGE ( 'NONE', *, *, #7773, .F. ) ;
#16862 = DIRECTION ( 'NONE',  ( -1.000000000000000000, -0.000000000000000000, -0.000000000000000000 ) ) ;
#16863 = ORIENTED_EDGE ( 'NONE', *, *, #22860, .T. ) ;
#16864 = AXIS2_PLACEMENT_3D ( 'NONE', #23361, #16072, #6966 ) ;
#16865 = CARTESIAN_POINT ( 'NONE',  ( 53.37731816583844591, 7.123453452023657206, 12.21969229848395599 ) ) ;
#16866 = PRESENTATION_LAYER_ASSIGNMENT (  '', '', ( #13049 ) ) ;
#16867 = CARTESIAN_POINT ( 'NONE',  ( 71.35000000109246798, 8.538419263543522320, 16.46158073645647235 ) ) ;
#16868 = DIRECTION ( 'NONE',  ( 0.000000000000000000, 0.9510565162951523099, 0.3090169943749515591 ) ) ;
#16869 = DIRECTION ( 'NONE',  ( 0.9396926207859107594, -0.3420201433256623291, 3.697785493223492838E-32 ) ) ;
#16870 = ORIENTED_EDGE ( 'NONE', *, *, #8663, .T. ) ;
#16871 = CARTESIAN_POINT ( 'NONE',  ( -3.999999999999999112, 1.656854249492380804, 15.06250000273119483 ) ) ;
#16872 = DIRECTION ( 'NONE',  ( 1.000000000000000000, 0.000000000000000000, 0.000000000000000000 ) ) ;
#16873 = CARTESIAN_POINT ( 'NONE',  ( 54.52893183416158962, 11.58880310854676132, 19.02818770551463956 ) ) ;
#16874 = CARTESIAN_POINT ( 'NONE',  ( 0.000000000000000000, 4.762163868918273479, 9.915734732513236338 ) ) ;
#16875 = DIRECTION ( 'NONE',  ( 0.000000000000000000, 0.000000000000000000, 1.000000000000000000 ) ) ;
#16876 = CIRCLE ( 'NONE', #17257, 11.00000000000000000 ) ;
#16877 = DIRECTION ( 'NONE',  ( 0.3420201433256622736, -0.9396926207859106484, -1.232595164407828100E-31 ) ) ;
#16878 = CARTESIAN_POINT ( 'NONE',  ( -19.99999999999999645, -9.000000000000003553, 10.00000000000008882 ) ) ;
#16879 = CARTESIAN_POINT ( 'NONE',  ( 3.250000000000002665, -5.629165124598850767, -3.700000000000000178 ) ) ;
#16880 = ORIENTED_EDGE ( 'NONE', *, *, #5850, .T. ) ;
#16881 = EDGE_CURVE ( 'NONE', #19202, #22418, #12654, .T. ) ;
#16882 = CARTESIAN_POINT ( 'NONE',  ( 53.15625000000000711, 7.000000000000002665, 16.24264068711929099 ) ) ;
#16883 = DIRECTION ( 'NONE',  ( -1.000000000000000000, -0.000000000000000000, -0.000000000000000000 ) ) ;
#16884 = EDGE_CURVE ( 'NONE', #660, #8473, #5764, .T. ) ;
#16885 = ADVANCED_FACE ( 'NONE', ( #5637 ), #9260, .T. ) ;
#16886 = ORIENTED_EDGE ( 'NONE', *, *, #1730, .T. ) ;
#16887 = DIRECTION ( 'NONE',  ( -1.000000000000000000, 0.000000000000000000, 1.224646799147353207E-16 ) ) ;
#16888 = CARTESIAN_POINT ( 'NONE',  ( -3.999999999999999112, 1.656854249492380582, 15.06250000273119660 ) ) ;
#16889 = DIRECTION ( 'NONE',  ( 0.000000000000000000, 0.000000000000000000, 1.000000000000000000 ) ) ;
#16890 = PLANE ( 'NONE',  #1041 ) ;
#16891 = ORIENTED_EDGE ( 'NONE', *, *, #3101, .F. ) ;
#16892 = DIRECTION ( 'NONE',  ( -1.000000000000000000, -0.000000000000000000, -0.000000000000000000 ) ) ;
#16893 = ORIENTED_EDGE ( 'NONE', *, *, #13877, .F. ) ;
#16894 = B_SPLINE_CURVE_WITH_KNOTS ( 'NONE', 3,
 ( #7755, #14830, #22084, #11118, #9557, #1976 ),
 .UNSPECIFIED., .F., .F.,
 ( 4, 2, 4 ),
 ( 0.002365888236227967761, 0.003551327329835077609, 0.004736766423442186590 ),
 .UNSPECIFIED. ) ;
#16895 = CARTESIAN_POINT ( 'NONE',  ( 4.000000000000000888, -1.656854249492379694, 1.737500000000001377 ) ) ;
#16896 = CARTESIAN_POINT ( 'NONE',  ( 9.920644283265380691E-16, 4.000000000000000000, 14.75000000000000888 ) ) ;
#16897 = CARTESIAN_POINT ( 'NONE',  ( -3.250000000000004441, 5.629165124598849879, -3.700000000000000178 ) ) ;
#16898 = CARTESIAN_POINT ( 'NONE',  ( 5.200000000000002842, 3.306546357697854226E-16, 2.700000000000000622 ) ) ;
#16899 = FACE_OUTER_BOUND ( 'NONE', #10665, .T. ) ;
#16900 = CARTESIAN_POINT ( 'NONE',  ( 70.75000000109247367, 8.538419263543522320, 16.46158073645647235 ) ) ;
#16901 = ORIENTED_EDGE ( 'NONE', *, *, #3894, .T. ) ;
#16902 = CARTESIAN_POINT ( 'NONE',  ( 4.623144047065553153, 4.836380039389420737, -0.1061556211655326765 ) ) ;
#16903 = CARTESIAN_POINT ( 'NONE',  ( 72.50000000000000000, 9.999999999999998224, 12.49999999999999289 ) ) ;
#16904 = CARTESIAN_POINT ( 'NONE',  ( 71.75000000109247367, 8.538419263543524096, 13.53841926354352054 ) ) ;
#16905 = CARTESIAN_POINT ( 'NONE',  ( 3.458734125000002102, -1.432654583217639610, 11.87500000136560452 ) ) ;
#16906 = CARTESIAN_POINT ( 'NONE',  ( 1.546713180332750293, -11.25000000000000355, 5.000000000000079936 ) ) ;
#16907 = CARTESIAN_POINT ( 'NONE',  ( 3.458734125000000770, 1.432654583217640498, -0.4499999986344046521 ) ) ;
#16909 = EDGE_CURVE ( 'NONE', #2194, #3058, #4, .T. ) ;
#16908 = CARTESIAN_POINT ( 'NONE',  ( -4.000000000000000888, 1.656854249492380804, 1.237500000000000933 ) ) ;
#16910 = CARTESIAN_POINT ( 'NONE',  ( -71.00000000218494733, 9.999999999999998224, 17.49999999999999645 ) ) ;
#16911 = CARTESIAN_POINT ( 'NONE',  ( 1.025207404391860050E-15, 3.458734125000000326, 13.18750000136560452 ) ) ;
#16912 = DIRECTION ( 'NONE',  ( 0.000000000000000000, -1.000000000000000000, 1.287488025362403787E-15 ) ) ;
#16913 = ORIENTED_EDGE ( 'NONE', *, *, #19484, .F. ) ;
#16914 = CARTESIAN_POINT ( 'NONE',  ( -65.90000000109247935, 7.933012699999995476, 14.14382582708705094 ) ) ;
#16915 = ORIENTED_EDGE ( 'NONE', *, *, #16513, .F. ) ;
#16916 = CARTESIAN_POINT ( 'NONE',  ( 58.59375000000000711, 11.65685424949236193, 10.99999999999998401 ) ) ;
#16917 = CARTESIAN_POINT ( 'NONE',  ( -71.75000000109247367, 8.538419263543524096, 13.53841926354352054 ) ) ;
#16918 = ITEM_DEFINED_TRANSFORMATION ( 'NONE', 'NONE', #3411,  #7318 ) ;
#16919 = ORIENTED_EDGE ( 'NONE', *, *, #17831, .F. ) ;
#16920 = DIRECTION ( 'NONE',  ( 7.087422195345011518E-32, 1.000000000000000000, -0.000000000000000000 ) ) ;
#16921 = ORIENTED_EDGE ( 'NONE', *, *, #9963, .F. ) ;
#16922 = VERTEX_POINT ( 'NONE', #12626 ) ;
#16923 = CARTESIAN_POINT ( 'NONE',  ( 2.445694354108822299, -2.445694354108820079, 15.06250000136560452 ) ) ;
#16924 = CARTESIAN_POINT ( 'NONE',  ( 55.40625000000000000, 12.99999999999999645, 13.75735931288070191 ) ) ;
#16925 = ADVANCED_FACE ( 'NONE', ( #13092 ), #9023, .T. ) ;
#16926 = CARTESIAN_POINT ( 'NONE',  ( -69.15000000109247935, 8.538419263543524096, 13.53841926354352054 ) ) ;
#16927 = CARTESIAN_POINT ( 'NONE',  ( 67.80000000109247082, 12.06698729999999919, 14.14382582708705094 ) ) ;
#16928 = CARTESIAN_POINT ( 'NONE',  ( -68.25000000109245946, 9.999999999999998224, 17.06698730000000097 ) ) ;
#16929 =( BOUNDED_CURVE ( )  B_SPLINE_CURVE ( 2, ( #5668, #13000, #16692, #18721, #2423, #20380, #18478, #20265, #3987 ),
 .UNSPECIFIED., .F., .F. ) 
 B_SPLINE_CURVE_WITH_KNOTS ( ( 3, 2, 2, 2, 3 ),
 ( 0.5625000000000008882, 0.5781250000000007772, 0.5937500000000006661, 0.6093750000000006661, 0.6250000000000005551 ),
 .UNSPECIFIED. ) 
 CURVE ( )  GEOMETRIC_REPRESENTATION_ITEM ( )  RATIONAL_B_SPLINE_CURVE ( ( 0.9999999999999956701, 0.9238795325112910684, 1.000000000000000000, 0.9238795325112867385, 1.000000000000000000, 0.9238795325112867385, 1.000000000000000000, 0.9238795325112840739, 1.000000000000002665 ) ) 
 REPRESENTATION_ITEM ( '' )  );
#16930 = PLANE ( 'NONE',  #8438 ) ;
#16931 = CARTESIAN_POINT ( 'NONE',  ( 57.71643183416158251, 12.97181229448535689, 16.31069182806490758 ) ) ;
#16932 = CARTESIAN_POINT ( 'NONE',  ( 1.546713180332750293, -11.25000000000000355, 5.000000000000079936 ) ) ;
#16933 = CARTESIAN_POINT ( 'NONE',  ( -3.458734125000000770, 0.000000000000000000, 3.987500001365595015 ) ) ;
#16934 = CARTESIAN_POINT ( 'NONE',  ( 3.458734125000001214, 1.432654583217640498, 11.00000000136560452 ) ) ;
#16935 = CARTESIAN_POINT ( 'NONE',  ( 4.000000000000000888, 4.898587196589412829E-16, 14.62500000273119660 ) ) ;
#16936 = CARTESIAN_POINT ( 'NONE',  ( 35.00000000000000000, 4.500000000000001776, -20.00000000000000355 ) ) ;
#16937 = ORIENTED_EDGE ( 'NONE', *, *, #5419, .T. ) ;
#16938 = CARTESIAN_POINT ( 'NONE',  ( -0.5449313310646672903, -4.304185902836978883, -3.316620875263469159 ) ) ;
#16939 = ORIENTED_EDGE ( 'NONE', *, *, #7871, .F. ) ;
#16940 = CARTESIAN_POINT ( 'NONE',  ( 58.84143183416158962, 8.689308171935088865, 17.97181229448535689 ) ) ;
#16941 =( NAMED_UNIT ( * ) PLANE_ANGLE_UNIT ( ) SI_UNIT ( $, .RADIAN. ) );
#16942 = CARTESIAN_POINT ( 'NONE',  ( -2.445694354108820523, 2.445694354108820523, 2.612500001365597235 ) ) ;
#16943 = DIRECTION ( 'NONE',  ( -1.000000000000000000, 0.000000000000000000, 0.000000000000000000 ) ) ;
#16944 = ORIENTED_EDGE ( 'NONE', *, *, #14235, .F. ) ;
#16945 = CARTESIAN_POINT ( 'NONE',  ( -2.828427124746189403, 2.828427124746190291, 11.87500000000001066 ) ) ;
#16946 = LINE ( 'NONE', #15168, #20179 ) ;
#16947 = CARTESIAN_POINT ( 'NONE',  ( -2.828427124746189403, 2.828427124746190291, 14.87500000000000888 ) ) ;
#16948 = EDGE_LOOP ( 'NONE', ( #1655, #14252 ) ) ;
#16949 = ADVANCED_FACE ( 'NONE', ( #1679 ), #3955, .T. ) ;
#16950 = CARTESIAN_POINT ( 'NONE',  ( -71.30000000218494449, 8.232233047033629347, 13.23223304703362402 ) ) ;
#16951 = CARTESIAN_POINT ( 'NONE',  ( 34.99999999999999289, 1.500000000000009992, -50.00000000000000711 ) ) ;
#16952 = CARTESIAN_POINT ( 'NONE',  ( 30.70991776966726405, -11.25000000000000355, 5.000000000000079936 ) ) ;
#16953 = CARTESIAN_POINT ( 'NONE',  ( 69.25000000000000000, 11.03553390593273598, 17.50000000000000355 ) ) ;
#16954 = EDGE_CURVE ( 'NONE', #3506, #2340, #11293, .T. ) ;
#16955 = CYLINDRICAL_SURFACE ( 'NONE', #9717, 2.500000000000002220 ) ;
#16956 = CARTESIAN_POINT ( 'NONE',  ( 0.000000000000000000, 0.000000000000000000, 0.000000000000000000 ) ) ;
#16957 = CARTESIAN_POINT ( 'NONE',  ( 57.78356816583844591, 8.689308171935074654, 12.02818770551464489 ) ) ;
#16958 = CARTESIAN_POINT ( 'NONE',  ( 6.353591512924457348E-16, -3.458734125000000770, 4.237500001365595459 ) ) ;
#16959 = CARTESIAN_POINT ( 'NONE',  ( 2.445694354108822299, -2.445694354108820079, 16.06250000136560629 ) ) ;
#16960 = CARTESIAN_POINT ( 'NONE',  ( -72.04999999999998295, 8.964466094067278235, 12.49999999999997691 ) ) ;
#16961 = DIRECTION ( 'NONE',  ( -0.5000000000000013323, -0.000000000000000000, 0.8660254037844380415 ) ) ;
#16962 = DIRECTION ( 'NONE',  ( 0.3420201433256622181, -0.9396926207859107594, 0.000000000000000000 ) ) ;
#16963 = EDGE_LOOP ( 'NONE', ( #9082, #13039, #7132, #23433 ) ) ;
#16964 = CARTESIAN_POINT ( 'NONE',  ( -1.656854249492380138, -3.999999999999999112, 14.18750000000001066 ) ) ;
#16965 = CYLINDRICAL_SURFACE ( 'NONE', #7942, 2.500000000000002220 ) ;
#16966 = CARTESIAN_POINT ( 'NONE',  ( -70.90000000109246514, 10.85617417291294551, 12.93301269999999370 ) ) ;
#16967 = VERTEX_POINT ( 'NONE', #14768 ) ;
#16968 =( REPRESENTATION_RELATIONSHIP ('NONE','NONE', #8403, #15757 ) REPRESENTATION_RELATIONSHIP_WITH_TRANSFORMATION ( #4444 )SHAPE_REPRESENTATION_RELATIONSHIP( ) );
#16969 = ORIENTED_EDGE ( 'NONE', *, *, #1321, .F. ) ;
#16970 =( LENGTH_UNIT ( ) NAMED_UNIT ( * ) SI_UNIT ( .MILLI., .METRE. ) );
#16971 = CARTESIAN_POINT ( 'NONE',  ( 60.00000000000000000, 9.999999999999998224, 14.99999999999999645 ) ) ;
#16972 = ORIENTED_EDGE ( 'NONE', *, *, #13747, .T. ) ;
#16973 = CARTESIAN_POINT ( 'NONE',  ( 44.09522139676619901, -9.000000000000003553, 10.00454388062671640 ) ) ;
#16974 = AXIS2_PLACEMENT_3D ( 'NONE', #20286, #7276, #172 ) ;
#16975 = UNCERTAINTY_MEASURE_WITH_UNIT (LENGTH_MEASURE( 1.000000000000000082E-05 ), #15045, 'distance_accuracy_value', 'NONE');
#16976 = EDGE_CURVE ( 'NONE', #2926, #4629, #10921, .T. ) ;
#16977 = EDGE_CURVE ( 'NONE', #21411, #8404, #6673, .T. ) ;
#16978 = CARTESIAN_POINT ( 'NONE',  ( 70.00000000109248788, 9.143825827087050939, 12.93301269999999370 ) ) ;
#16979 = LINE ( 'NONE', #18411, #9987 ) ;
#16980 = ORIENTED_EDGE ( 'NONE', *, *, #9696, .T. ) ;
#16981 = CARTESIAN_POINT ( 'NONE',  ( 71.65000000109246514, 7.933012699999995476, 14.99999999999999645 ) ) ;
#16982 = ADVANCED_FACE ( 'NONE', ( #3842 ), #13555, .F. ) ;
#16983 = PRODUCT ( 'Gripper Jaw with Integrated Rack', 'Gripper Jaw with Integrated Rack', '', ( #16794 ) ) ;
#16984 = ORIENTED_EDGE ( 'NONE', *, *, #23128, .F. ) ;
#16985 = CARTESIAN_POINT ( 'NONE',  ( -2.828427124746188515, -2.828427124746190735, 12.25000000273119838 ) ) ;
#16986 = EDGE_CURVE ( 'NONE', #4647, #11669, #15012, .T. ) ;
#16987 = CYLINDRICAL_SURFACE ( 'NONE', #20610, 4.000000000000000000 ) ;
#16988 = CARTESIAN_POINT ( 'NONE',  ( 55.46643183416158962, 6.028187705514633343, 13.27509460956200016 ) ) ;
#16989 = CARTESIAN_POINT ( 'NONE',  ( 71.40000000218495302, 9.999999999999998224, 12.49999999999999289 ) ) ;
#16990 = FACE_OUTER_BOUND ( 'NONE', #4951, .T. ) ;
#16991 = PLANE ( 'NONE',  #3244 ) ;
#16992 = CARTESIAN_POINT ( 'NONE',  ( 2.499999999999999556, 7.958834565716766285, 7.593217523260609170 ) ) ;
#16993 = EDGE_LOOP ( 'NONE', ( #12986, #15925, #2628, #23377 ) ) ;
#16994 = CARTESIAN_POINT ( 'NONE',  ( -6.500000000000000000, 3.752776749732573247, -3.119443416399232394 ) ) ;
#16995 = ORIENTED_EDGE ( 'NONE', *, *, #19514, .T. ) ;
#16996 = CARTESIAN_POINT ( 'NONE',  ( 51.56250000000000711, 6.999999999999997335, 15.00000000000000533 ) ) ;
#16997 = CARTESIAN_POINT ( 'NONE',  ( 46.41788101966725577, -11.25000000000000355, 5.000000000000079936 ) ) ;
#16998 = VERTEX_POINT ( 'NONE', #483 ) ;
#16999 = LINE ( 'NONE', #20446, #21982 ) ;
#17000 = DIRECTION ( 'NONE',  ( -0.000000000000000000, -1.000000000000000000, -0.000000000000000000 ) ) ;
#17001 = DIRECTION ( 'NONE',  ( -1.224646799147353454E-16, 0.000000000000000000, -1.000000000000000000 ) ) ;
#17002 = DIRECTION ( 'NONE',  ( 0.000000000000000000, 0.000000000000000000, 1.000000000000000000 ) ) ;
#17003 = ORIENTED_EDGE ( 'NONE', *, *, #22423, .T. ) ;
#17004 = DIRECTION ( 'NONE',  ( -0.000000000000000000, 1.000000000000000000, -0.000000000000000000 ) ) ;
#17005 = ORIENTED_EDGE ( 'NONE', *, *, #8238, .T. ) ;
#17006 = DIRECTION ( 'NONE',  ( 1.000000000000000000, 0.000000000000000000, 0.000000000000000000 ) ) ;
#17007 = ADVANCED_FACE ( 'NONE', ( #18919 ), #6117, .F. ) ;
#17008 = CARTESIAN_POINT ( 'NONE',  ( -1.656854249492379250, 4.000000000000000000, 12.81250000000001066 ) ) ;
#17009 = PLANE ( 'NONE',  #3834 ) ;
#17010 = CARTESIAN_POINT ( 'NONE',  ( 25.25491034071656316, -8.974600000000002353, 10.00000000000008882 ) ) ;
#17011 = DIRECTION ( 'NONE',  ( 0.3420201433256622736, 0.9396926207859106484, 0.000000000000000000 ) ) ;
#17012 = CARTESIAN_POINT ( 'NONE',  ( 69.95000000109247651, 8.538419263543522320, 16.46158073645647235 ) ) ;
#17013 = VERTEX_POINT ( 'NONE', #7920 ) ;
#17014 = EDGE_CURVE ( 'NONE', #21452, #5142, #556, .T. ) ;
#17015 = DIRECTION ( 'NONE',  ( -1.000000000000000000, 0.000000000000000000, -0.000000000000000000 ) ) ;
#17016 = CARTESIAN_POINT ( 'NONE',  ( 4.999999999999999112, 0.000000000000000000, 0.000000000000000000 ) ) ;
#17017 = CARTESIAN_POINT ( 'NONE',  ( 65.95000000109247651, 8.538419263543524096, 13.53841926354352054 ) ) ;
#17018 = CARTESIAN_POINT ( 'NONE',  ( 3.458734125000001214, 4.235727675282971730E-16, 14.93750000136560452 ) ) ;
#17019 = CARTESIAN_POINT ( 'NONE',  ( 50.00000000000000000, 15.00000000000001954, 10.00000000000008882 ) ) ;
#17020 = CIRCLE ( 'NONE', #14348, 4.000000000000002665 ) ;
#17021 = FACE_BOUND ( 'NONE', #17849, .T. ) ;
#17022 = CARTESIAN_POINT ( 'NONE',  ( 2.828427124746190735, -2.828427124746189847, -0.3249999999999971800 ) ) ;
#17023 = CARTESIAN_POINT ( 'NONE',  ( -2.828427124746189403, -2.828427124746190735, -3.449999997268813345 ) ) ;
#17024 = VECTOR ( 'NONE', #2745, 1000.000000000000000 ) ;
#17025 = LINE ( 'NONE', #599, #6638 ) ;
#17026 = LINE ( 'NONE', #9976, #9993 ) ;
#17027 = ORIENTED_EDGE ( 'NONE', *, *, #20202, .T. ) ;
#17028 = CARTESIAN_POINT ( 'NONE',  ( 9.920644283265380691E-16, 4.000000000000000000, 15.87500000273119660 ) ) ;
#17029 = ORIENTED_EDGE ( 'NONE', *, *, #6733, .T. ) ;
#17030 = CARTESIAN_POINT ( 'NONE',  ( 55.78125000000000000, 8.343145750507600766, 11.00000000000000533 ) ) ;
#17031 = CARTESIAN_POINT ( 'NONE',  ( -70.25000000109245946, 9.999999999999998224, 12.93301269999999192 ) ) ;
#17032 = PRODUCT_CONTEXT ( 'NONE', #12233, 'mechanical' ) ;
#17033 = ORIENTED_EDGE ( 'NONE', *, *, #5266, .F. ) ;
#17034 = CARTESIAN_POINT ( 'NONE',  ( 0.000000000000000000, 1.239665997526886665, 9.314797388894895391 ) ) ;
#17035 = ORIENTED_EDGE ( 'NONE', *, *, #7610, .F. ) ;
#17036 = ORIENTED_EDGE ( 'NONE', *, *, #5590, .T. ) ;
#17037 = CARTESIAN_POINT ( 'NONE',  ( -2.445694354108819191, 2.445694354108820523, 15.56250000136560629 ) ) ;
#17038 = CARTESIAN_POINT ( 'NONE',  ( 57.65625000000002132, 7.000000000000003553, 16.24264068711929099 ) ) ;
#17039 = ORIENTED_EDGE ( 'NONE', *, *, #3363, .T. ) ;
#17040 = VECTOR ( 'NONE', #18664, 1000.000000000000114 ) ;
#17041 = CARTESIAN_POINT ( 'NONE',  ( -68.75000000109247367, 11.46158073645647235, 16.46158073645647235 ) ) ;
#17042 = VECTOR ( 'NONE', #19826, 1000.000000000000114 ) ;
#17043 = CARTESIAN_POINT ( 'NONE',  ( 69.80000000109247082, 7.933012699999995476, 15.85617417291294196 ) ) ;
#17044 = EDGE_CURVE ( 'NONE', #17175, #9561, #2845, .T. ) ;
#17045 = CARTESIAN_POINT ( 'NONE',  ( -72.39999999999999147, 11.76776695296636888, 16.76776695296636532 ) ) ;
#17046 = DIRECTION ( 'NONE',  ( 1.000000000000000000, 0.000000000000000000, 0.000000000000000000 ) ) ;
#17047 = CARTESIAN_POINT ( 'NONE',  ( 54.34143183416158251, 8.689308171935088865, 17.97181229448535689 ) ) ;
#17048 = DIRECTION ( 'NONE',  ( 1.000000000000000000, 0.000000000000000000, 0.000000000000000000 ) ) ;
#17049 = CARTESIAN_POINT ( 'NONE',  ( -1.432654583217641164, -3.458734125000000326, 4.175000001365593683 ) ) ;
#17050 = LINE ( 'NONE', #4341, #19660 ) ;
#17051 = CARTESIAN_POINT ( 'NONE',  ( 1.971781867644420635E-15, -4.000000000000000000, 13.37500000273119660 ) ) ;
#17052 = CARTESIAN_POINT ( 'NONE',  ( 0.000000000000000000, 9.314797388894893615, 5.239665997526921082 ) ) ;
#17053 = ORIENTED_EDGE ( 'NONE', *, *, #14504, .F. ) ;
#17054 = CARTESIAN_POINT ( 'NONE',  ( -3.999999999999999112, 0.000000000000000000, 14.00000000000001066 ) ) ;
#17055 = VERTEX_POINT ( 'NONE', #20709 ) ;
#17056 = CARTESIAN_POINT ( 'NONE',  ( 59.12268183416157541, 12.07320092032950676, 17.16943976678977180 ) ) ;
#17057 = CIRCLE ( 'NONE', #6726, 2.649999999999992806 ) ;
#17058 =( NAMED_UNIT ( * ) SI_UNIT ( $, .STERADIAN. ) SOLID_ANGLE_UNIT ( ) );
#17059 = CARTESIAN_POINT ( 'NONE',  ( 1.432654583217639832, 3.458734125000000326, 0.4250000013655961251 ) ) ;
#17060 = AXIS2_PLACEMENT_3D ( 'NONE', #10775, #5224, #10882 ) ;
#17061 = CARTESIAN_POINT ( 'NONE',  ( 6.353591512924457348E-16, -3.458734125000000326, -0.01249999863440348635 ) ) ;
#17062 = ORIENTED_EDGE ( 'NONE', *, *, #4266, .F. ) ;
#17063 = CARTESIAN_POINT ( 'NONE',  ( 1.656854249492381470, 4.000000000000000000, 12.68750000000001243 ) ) ;
#17064 = CARTESIAN_POINT ( 'NONE',  ( -3.999999999999999112, 0.000000000000000000, 15.00000000000001066 ) ) ;
#17065 = VERTEX_POINT ( 'NONE', #18687 ) ;
#17066 = VECTOR ( 'NONE', #17624, 1000.000000000000000 ) ;
#17067 = CARTESIAN_POINT ( 'NONE',  ( -71.15000000218493881, 7.499999999999995559, 16.03553390593273420 ) ) ;
#17068 =( BOUNDED_CURVE ( )  B_SPLINE_CURVE ( 2, ( #17054, #10239, #17530, #6033, #4462, #11684, #13359, #17297, #10009 ),
 .UNSPECIFIED., .F., .F. ) 
 B_SPLINE_CURVE_WITH_KNOTS ( ( 3, 2, 2, 2, 3 ),
 ( 0.5999999999999999778, 0.6125000000000000444, 0.6250000000000000000, 0.6374999999999999556, 0.6500000000000000222 ),
 .UNSPECIFIED. ) 
 CURVE ( )  GEOMETRIC_REPRESENTATION_ITEM ( )  RATIONAL_B_SPLINE_CURVE ( ( 1.000000000000000000, 0.9238795325112867385, 1.000000000000000000, 0.9238795325112867385, 1.000000000000000000, 0.9238795325112867385, 1.000000000000000000, 0.9238795325112867385, 1.000000000000000000 ) ) 
 REPRESENTATION_ITEM ( '' )  );
#17069 = CARTESIAN_POINT ( 'NONE',  ( -3.458734125000000770, 0.000000000000000000, -2.012499998634403653 ) ) ;
#17070 = CARTESIAN_POINT ( 'NONE',  ( 1.567478505476134606E-15, 4.618802153517012066, -3.433295621305382905 ) ) ;
#17071 = DIRECTION ( 'NONE',  ( -1.000000000000000000, 0.000000000000000000, -0.000000000000000000 ) ) ;
#17072 = CARTESIAN_POINT ( 'NONE',  ( -71.24999999999998579, 8.964466094067205404, 12.50000000000004263 ) ) ;
#17073 = CARTESIAN_POINT ( 'NONE',  ( 69.50000000109248788, 12.06698730000000275, 15.85617417291294196 ) ) ;
#17074 = CARTESIAN_POINT ( 'NONE',  ( -2.000000000000006661, 3.464101615137750834, 0.000000000000000000 ) ) ;
#17075 = CARTESIAN_POINT ( 'NONE',  ( 54.22106816583844591, 13.02818770551464489, 16.17458954617363531 ) ) ;
#17076 = CARTESIAN_POINT ( 'NONE',  ( -2.445694354108820523, 2.445694354108820523, -2.387499998634403653 ) ) ;
#17077 = CARTESIAN_POINT ( 'NONE',  ( -2.445694354108819191, 2.445694354108820523, 14.56250000136560452 ) ) ;
#17078 = PLANE ( 'NONE',  #17210 ) ;
#17079 = CARTESIAN_POINT ( 'NONE',  ( -70.75000000109247367, 8.538419263543522320, 16.46158073645647235 ) ) ;
#17080 = EDGE_CURVE ( 'NONE', #1856, #23288, #20935, .T. ) ;
#17081 = LINE ( 'NONE', #654, #16620 ) ;
#17082 = ORIENTED_EDGE ( 'NONE', *, *, #15476, .F. ) ;
#17083 = DIRECTION ( 'NONE',  ( -1.000000000000000000, -0.000000000000000000, -0.000000000000000000 ) ) ;
#17084 = CARTESIAN_POINT ( 'NONE',  ( 4.000000000000000000, 4.898587196589412829E-16, 3.925000002731186655 ) ) ;
#17085 = CARTESIAN_POINT ( 'NONE',  ( -71.95000000109247651, 11.46158073645647235, 16.46158073645647235 ) ) ;
#17086 = ORIENTED_EDGE ( 'NONE', *, *, #20831, .T. ) ;
#17087 = ORIENTED_EDGE ( 'NONE', *, *, #15860, .T. ) ;
#17088 = FACE_OUTER_BOUND ( 'NONE', #12146, .T. ) ;
#17089 = EDGE_CURVE ( 'NONE', #5711, #10249, #10085, .T. ) ;
#17090 = CARTESIAN_POINT ( 'NONE',  ( 69.70000000000000284, 9.999999999999998224, 12.49999999999999289 ) ) ;
#17091 = VERTEX_POINT ( 'NONE', #22267 ) ;
#17092 = CARTESIAN_POINT ( 'NONE',  ( 44.00000000000000711, -9.261618637464055226, 10.00000000000008882 ) ) ;
#17093 = CARTESIAN_POINT ( 'NONE',  ( 69.75000000109247367, 8.538419263543522320, 16.46158073645647235 ) ) ;
#17094 = CARTESIAN_POINT ( 'NONE',  ( 71.35000000109246798, 11.46158073645647235, 16.46158073645647235 ) ) ;
#17095 = ORIENTED_EDGE ( 'NONE', *, *, #14379, .T. ) ;
#17096 =( BOUNDED_CURVE ( )  B_SPLINE_CURVE ( 2, ( #10542, #3086, #3196, #4882, #6685, #19488, #8726, #17819, #23190 ),
 .UNSPECIFIED., .F., .F. ) 
 B_SPLINE_CURVE_WITH_KNOTS ( ( 3, 2, 2, 2, 3 ),
 ( 0.7499999999999997780, 0.7656249999999996669, 0.7812499999999995559, 0.7968749999999994449, 0.8124999999999993339 ),
 .UNSPECIFIED. ) 
 CURVE ( )  GEOMETRIC_REPRESENTATION_ITEM ( )  RATIONAL_B_SPLINE_CURVE ( ( 1.000000000000001110, 0.9238795325112856283, 1.000000000000000000, 0.9238795325112867385, 1.000000000000000000, 0.9238795325112867385, 1.000000000000000000, 0.9238795325112899581, 0.9999999999999967804 ) ) 
 REPRESENTATION_ITEM ( '' )  );
#17097 = DIRECTION ( 'NONE',  ( -1.000000000000000000, 0.000000000000000000, 0.000000000000000000 ) ) ;
#17098 = CARTESIAN_POINT ( 'NONE',  ( 55.78125000000000000, 8.343145750507600766, 11.00000000000000533 ) ) ;
#17099 = DIRECTION ( 'NONE',  ( -1.000000000000000000, -7.703719777548943412E-32, 0.000000000000000000 ) ) ;
#17100 = CARTESIAN_POINT ( 'NONE',  ( 66.70000000218495018, 11.76776695296636888, 13.23223304703362579 ) ) ;
#17101 = DIRECTION ( 'NONE',  ( 1.000000000000000000, 7.703719777548943412E-32, 0.000000000000000000 ) ) ;
#17102 = APPLICATION_CONTEXT ( 'automotive_design' ) ;
#17103 = ADVANCED_FACE ( 'NONE', ( #4197 ), #7807, .T. ) ;
#17104 = CARTESIAN_POINT ( 'NONE',  ( -66.40000000109247935, 12.06698729999999919, 14.14382582708705094 ) ) ;
#17105 = ORIENTED_EDGE ( 'NONE', *, *, #22673, .F. ) ;
#17106 = CARTESIAN_POINT ( 'NONE',  ( 3.860127959283449428, -8.974600000000002353, 5.000000000000079936 ) ) ;
#17107 = VERTEX_POINT ( 'NONE', #11539 ) ;
#17108 = ADVANCED_FACE ( 'NONE', ( #9841 ), #7473, .T. ) ;
#17109 = CARTESIAN_POINT ( 'NONE',  ( 3.263761790716562139, -8.974600000000002353, 5.000000000000079936 ) ) ;
#17110 = CARTESIAN_POINT ( 'NONE',  ( -19.99999999999999645, -9.000000000000003553, 5.000000000000079936 ) ) ;
#17111 = AXIS2_PLACEMENT_3D ( 'NONE', #13534, #17356, #2726 ) ;
#17112 = VECTOR ( 'NONE', #11218, 1000.000000000000000 ) ;
#17113 = ORIENTED_EDGE ( 'NONE', *, *, #8478, .T. ) ;
#17114 = CARTESIAN_POINT ( 'NONE',  ( 2.499999999999999556, -7.593217523260523016, -7.958834565716849774 ) ) ;
#17115 = CARTESIAN_POINT ( 'NONE',  ( 31.53809564071656624, -8.974600000000002353, 5.000000000000079936 ) ) ;
#17116 = CARTESIAN_POINT ( 'NONE',  ( 0.000000000000000000, 0.000000000000000000, 0.000000000000000000 ) ) ;
#17117 = EDGE_CURVE ( 'NONE', #5926, #4915, #1698, .T. ) ;
#17118 = LINE ( 'NONE', #925, #14462 ) ;
#17119 = ORIENTED_EDGE ( 'NONE', *, *, #15388, .T. ) ;
#17120 = CARTESIAN_POINT ( 'NONE',  ( 1.236993788156008760E-15, 0.000000000000000000, 21.31370849898476649 ) ) ;
#17121 = EDGE_LOOP ( 'NONE', ( #7007, #18131, #6388, #9957 ) ) ;
#17122 = CARTESIAN_POINT ( 'NONE',  ( 71.55000000109247082, 8.538419263543524096, 13.53841926354352054 ) ) ;
#17123 = CARTESIAN_POINT ( 'NONE',  ( 2.828427124746192067, -2.828427124746189847, 13.37500000000001243 ) ) ;
#17124 = CARTESIAN_POINT ( 'NONE',  ( 71.50000000218496155, 11.76776695296636888, 13.23223304703362579 ) ) ;
#17125 = AXIS2_PLACEMENT_3D ( 'NONE', #14070, #21335, #4956 ) ;
#17126 = CARTESIAN_POINT ( 'NONE',  ( 6.500000000000000888, 0.000000000000000000, -3.700000000000000178 ) ) ;
#17127 = CARTESIAN_POINT ( 'NONE',  ( -20.00000000000000711, -10.00000000000000000, -19.99999999999999645 ) ) ;
#17128 = CARTESIAN_POINT ( 'NONE',  ( 72.15000000109246514, 11.46158073645647235, 16.46158073645647235 ) ) ;
#17129 = ORIENTED_EDGE ( 'NONE', *, *, #15308, .T. ) ;
#17130 = CIRCLE ( 'NONE', #13315, 4.000000000000001776 ) ;
#17131 = AXIS2_PLACEMENT_3D ( 'NONE', #10309, #15697, #8609 ) ;
#17132 = FACE_OUTER_BOUND ( 'NONE', #9031, .T. ) ;
#17133 = EDGE_CURVE ( 'NONE', #5469, #6601, #6693, .T. ) ;
#17134 = LINE ( 'NONE', #9966, #22118 ) ;
#17135 = CARTESIAN_POINT ( 'NONE',  ( 71.30000000109247082, 12.06698730000000275, 15.85617417291294196 ) ) ;
#17136 = CARTESIAN_POINT ( 'NONE',  ( 1.872352939448454495E-15, -3.458734125000000326, 12.68750000136560629 ) ) ;
#17137 = DIRECTION ( 'NONE',  ( 1.000000000000000000, 0.000000000000000000, 1.040834085586083271E-15 ) ) ;
#17138 = DIRECTION ( 'NONE',  ( -1.000000000000000000, 0.000000000000000000, -0.000000000000000000 ) ) ;
#17139 = ORIENTED_EDGE ( 'NONE', *, *, #4702, .F. ) ;
#17140 = CARTESIAN_POINT ( 'NONE',  ( -4.000000000000000000, -1.656854249492383246, 1.362500000000001155 ) ) ;
#17141 = EDGE_CURVE ( 'NONE', #3286, #20917, #18809, .T. ) ;
#17142 = LINE ( 'NONE', #2749, #22393 ) ;
#17143 = CARTESIAN_POINT ( 'NONE',  ( -3.458734124999998993, 0.000000000000000000, 10.43750000136560452 ) ) ;
#17144 = CARTESIAN_POINT ( 'NONE',  ( 0.000000000000000000, 0.000000000000000000, -3.700000000000000178 ) ) ;
#17145 = ORIENTED_EDGE ( 'NONE', *, *, #18327, .F. ) ;
#17146 = AXIS2_PLACEMENT_3D ( 'NONE', #21423, #21897, #10459 ) ;
#17147 = CARTESIAN_POINT ( 'NONE',  ( -65.85000000109248219, 7.933012699999995476, 14.99999999999999645 ) ) ;
#17148 = VERTEX_POINT ( 'NONE', #19036 ) ;
#17149 = CARTESIAN_POINT ( 'NONE',  ( 59.34375000000000711, 8.343145750507638070, 19.00000000000000711 ) ) ;
#17150 = CARTESIAN_POINT ( 'NONE',  ( -67.90000000109245093, 10.85617417291294551, 12.93301269999999370 ) ) ;
#17151 = ADVANCED_FACE ( 'NONE', ( #7696 ), #20469, .F. ) ;
#17152 = ORIENTED_EDGE ( 'NONE', *, *, #21526, .T. ) ;
#17153 = DIRECTION ( 'NONE',  ( 0.000000000000000000, 1.224646799147333486E-16, 1.000000000000000000 ) ) ;
#17154 = ORIENTED_EDGE ( 'NONE', *, *, #9186, .F. ) ;
#17155 = AXIS2_PLACEMENT_3D ( 'NONE', #7738, #11694, #5925 ) ;
#17156 = EDGE_CURVE ( 'NONE', #3825, #14828, #2276, .T. ) ;
#17157 = ORIENTED_EDGE ( 'NONE', *, *, #16827, .F. ) ;
#17158 = CARTESIAN_POINT ( 'NONE',  ( 3.458734125000002546, -1.432654583217639610, 18.12500000136560274 ) ) ;
#17159 = CARTESIAN_POINT ( 'NONE',  ( 56.62500000000000000, 12.12132034355964727, 17.12132034355963484 ) ) ;
#17160 = CARTESIAN_POINT ( 'NONE',  ( -68.70000000109246230, 12.06698730000000275, 15.85617417291294196 ) ) ;
#17161 = CARTESIAN_POINT ( 'NONE',  ( 70.35000000109248219, 11.46158073645647235, 16.46158073645647235 ) ) ;
#17162 = VECTOR ( 'NONE', #18210, 1000.000000000000000 ) ;
#17163 = CARTESIAN_POINT ( 'NONE',  ( -66.75000000109245946, 8.538419263543522320, 16.46158073645647235 ) ) ;
#17164 = FACE_OUTER_BOUND ( 'NONE', #9981, .T. ) ;
#17165 = CARTESIAN_POINT ( 'NONE',  ( 58.37268183416157541, 7.926799079670491466, 12.83056023321021755 ) ) ;
#17166 = DIRECTION ( 'NONE',  ( 1.000000000000000000, 0.000000000000000000, 0.000000000000000000 ) ) ;
#17167 = AXIS2_PLACEMENT_3D ( 'NONE', #340, #7676, #464 ) ;
#17168 = AXIS2_PLACEMENT_3D ( 'NONE', #1521, #21152, #1984 ) ;
#17169 = CARTESIAN_POINT ( 'NONE',  ( -2.117863837641485618E-16, 3.458734125000000770, 3.737500001365594571 ) ) ;
#17170 = CARTESIAN_POINT ( 'NONE',  ( 2.445694354108821855, -2.445694354108820079, 11.81250000136560629 ) ) ;
#17171 = CARTESIAN_POINT ( 'NONE',  ( -2.828427124746189403, 2.828427124746190291, 13.00000000273119660 ) ) ;
#17172 = DIRECTION ( 'NONE',  ( -1.000000000000000000, -7.703719777548943412E-32, 0.000000000000000000 ) ) ;
#17173 = ORIENTED_EDGE ( 'NONE', *, *, #3476, .T. ) ;
#17174 = LINE ( 'NONE', #22419, #7845 ) ;
#17175 = VERTEX_POINT ( 'NONE', #15240 ) ;
#17176 = CARTESIAN_POINT ( 'NONE',  ( 60.90393183416158962, 13.02818770551463778, 13.82541045382633982 ) ) ;
#17177 = FILL_AREA_STYLE ('',( #22903 ) ) ;
#17178 = CARTESIAN_POINT ( 'NONE',  ( 3.458734125000000770, -1.432654583217639610, 1.175000001365597013 ) ) ;
#17180 = EDGE_CURVE ( 'NONE', #10717, #17305, #8244, .T. ) ;
#17179 = CIRCLE ( 'NONE', #3016, 2.500000000000002220 ) ;
#17181 = CARTESIAN_POINT ( 'NONE',  ( 1.432654583217642053, -3.458734124999999437, 1.050000001365596791 ) ) ;
#17182 = ORIENTED_EDGE ( 'NONE', *, *, #1139, .T. ) ;
#17183 = CARTESIAN_POINT ( 'NONE',  ( 2.828427124746192067, -2.828427124746189847, 14.37500000000001066 ) ) ;
#17184 = EDGE_CURVE ( 'NONE', #18995, #4822, #9970, .T. ) ;
#17185 = VECTOR ( 'NONE', #3326, 1000.000000000000000 ) ;
#17186 = DIRECTION ( 'NONE',  ( -1.000000000000000000, 0.000000000000000000, -0.000000000000000000 ) ) ;
#17187 = CARTESIAN_POINT ( 'NONE',  ( 1.656854249492381470, 4.000000000000000000, 14.68750000000000888 ) ) ;
#17188 = ORIENTED_EDGE ( 'NONE', *, *, #9524, .T. ) ;
#17189 = PRODUCT_DEFINITION_SHAPE ( 'NONE', 'NONE',  #23717 ) ;
#17190 = CARTESIAN_POINT ( 'NONE',  ( -69.80000000218494449, 9.999999999999998224, 12.49999999999999289 ) ) ;
#17191 = VECTOR ( 'NONE', #16008, 1000.000000000000000 ) ;
#17192 = LINE ( 'NONE', #16951, #22452 ) ;
#17193 = DIRECTION ( 'NONE',  ( -0.000000000000000000, -1.000000000000000000, -0.000000000000000000 ) ) ;
#17194 = CARTESIAN_POINT ( 'NONE',  ( 66.44999999999998863, 8.964466094067258695, 12.49999999999999289 ) ) ;
#17195 = AXIS2_PLACEMENT_3D ( 'NONE', #2496, #11645, #18801 ) ;
#17196 = CARTESIAN_POINT ( 'NONE',  ( -2.828427124746188515, -2.828427124746190735, 11.12500000000001066 ) ) ;
#17197 = CARTESIAN_POINT ( 'NONE',  ( 70.30000000109248504, 12.06698730000000275, 15.85617417291294196 ) ) ;
#17198 = CIRCLE ( 'NONE', #15675, 4.999999999999999112 ) ;
#17199 = CARTESIAN_POINT ( 'NONE',  ( 4.000000000000000000, 2.309401076758515803, -0.4999999999999995559 ) ) ;
#17200 = CARTESIAN_POINT ( 'NONE',  ( 54.03356816583844591, 11.31069182806492712, 17.97181229448534623 ) ) ;
#17201 = CARTESIAN_POINT ( 'NONE',  ( 3.458734125000001214, -1.432654583217639610, 5.425000001365595459 ) ) ;
#17202 = CARTESIAN_POINT ( 'NONE',  ( -3.458734124999999437, 1.432654583217640498, 10.62500000136560452 ) ) ;
#17203 = LINE ( 'NONE', #5817, #2486 ) ;
#17204 = ORIENTED_EDGE ( 'NONE', *, *, #14521, .F. ) ;
#17205 = CARTESIAN_POINT ( 'NONE',  ( -70.05000000218494449, 12.50000000000000000, 16.03553390593273775 ) ) ;
#17206 = DIRECTION ( 'NONE',  ( -1.000000000000000000, -7.703719777548943412E-32, 0.000000000000000000 ) ) ;
#17207 = ORIENTED_EDGE ( 'NONE', *, *, #9262, .F. ) ;
#17208 = CARTESIAN_POINT ( 'NONE',  ( 4.000000000000000000, 0.000000000000000000, 0.000000000000000000 ) ) ;
#17210 = AXIS2_PLACEMENT_3D ( 'NONE', #9550, #9311, #652 ) ;
#17209 =( NAMED_UNIT ( * ) PLANE_ANGLE_UNIT ( ) SI_UNIT ( $, .RADIAN. ) );
#17211 = CARTESIAN_POINT ( 'NONE',  ( 4.000000000000000888, -1.656854249492379694, 3.862500002731187543 ) ) ;
#17212 = CARTESIAN_POINT ( 'NONE',  ( -69.50000000109248788, 12.06698730000000275, 15.85617417291294196 ) ) ;
#17213 = ORIENTED_EDGE ( 'NONE', *, *, #18986, .F. ) ;
#17214 = ORIENTED_EDGE ( 'NONE', *, *, #15350, .F. ) ;
#17215 = CARTESIAN_POINT ( 'NONE',  ( -1.144235203016679359, -3.958177651039096911, -0.09382832055446428676 ) ) ;
#17216 =( BOUNDED_CURVE ( )  B_SPLINE_CURVE ( 2, ( #1012, #22935, #17563, #15663, #1127, #19335, #21236, #6549, #4848 ),
 .UNSPECIFIED., .F., .F. ) 
 B_SPLINE_CURVE_WITH_KNOTS ( ( 3, 2, 2, 2, 3 ),
 ( 0.3499999999999999778, 0.3624999999999999889, 0.3750000000000000000, 0.3875000000000000111, 0.4000000000000000222 ),
 .UNSPECIFIED. ) 
 CURVE ( )  GEOMETRIC_REPRESENTATION_ITEM ( )  RATIONAL_B_SPLINE_CURVE ( ( 1.000000000000000000, 0.9238795325112867385, 1.000000000000000000, 0.9238795325112867385, 1.000000000000000000, 0.9238795325112867385, 1.000000000000000000, 0.9238795325112867385, 1.000000000000000000 ) ) 
 REPRESENTATION_ITEM ( '' )  );
#17217 = CARTESIAN_POINT ( 'NONE',  ( 51.09375000000000711, 11.65685424949236015, 10.99999999999998579 ) ) ;
#17218 = ORIENTED_EDGE ( 'NONE', *, *, #21059, .T. ) ;
#17219 = CARTESIAN_POINT ( 'NONE',  ( 2.807080416178989513, -3.225969019225150003, -3.502507215260505014 ) ) ;
#17220 = CIRCLE ( 'NONE', #1889, 7.000000000000000000 ) ;
#17221 = UNCERTAINTY_MEASURE_WITH_UNIT (LENGTH_MEASURE( 1.000000000000000082E-05 ), #19944, 'distance_accuracy_value', 'NONE');
#17222 = CARTESIAN_POINT ( 'NONE',  ( 68.80000000109247082, 10.85617417291294551, 17.06698729999999742 ) ) ;
#17223 = AXIS2_PLACEMENT_3D ( 'NONE', #13769, #8374, #18785 ) ;
#17224 = EDGE_CURVE ( 'NONE', #2372, #8909, #12001, .T. ) ;
#17225 = VECTOR ( 'NONE', #14209, 1000.000000000000000 ) ;
#17226 = CARTESIAN_POINT ( 'NONE',  ( 68.80000000109247082, 12.06698730000000275, 14.14382582708705094 ) ) ;
#17227 = VERTEX_POINT ( 'NONE', #17493 ) ;
#17228 = DIRECTION ( 'NONE',  ( 6.779273404243053781E-32, 0.9396926207859083169, -0.3420201433256691015 ) ) ;
#17229 = CARTESIAN_POINT ( 'NONE',  ( 57.28125000000000711, 8.343145750507600766, 11.00000000000000533 ) ) ;
#17230 = CARTESIAN_POINT ( 'NONE',  ( 71.80000000218494449, 9.999999999999998224, 17.49999999999999645 ) ) ;
#17231 = DIRECTION ( 'NONE',  ( 0.000000000000000000, 0.7071067811865414665, -0.7071067811865536790 ) ) ;
#17232 = CIRCLE ( 'NONE', #14564, 2.500000000000002220 ) ;
#17233 = FACE_OUTER_BOUND ( 'NONE', #10780, .T. ) ;
#17234 = CARTESIAN_POINT ( 'NONE',  ( 4.999999999999999112, -1.239665997526951724, 9.314797388894888286 ) ) ;
#17235 = ORIENTED_EDGE ( 'NONE', *, *, #6167, .T. ) ;
#17236 = CARTESIAN_POINT ( 'NONE',  ( 50.00000000000000711, -15.00000000000001954, 5.000000000000079936 ) ) ;
#17237 = CARTESIAN_POINT ( 'NONE',  ( -3.999999999999998224, -1.656854249492383024, 12.06250000000001066 ) ) ;
#17238 = CARTESIAN_POINT ( 'NONE',  ( -70.70000000000000284, 12.50000000000000000, 14.99999999999999645 ) ) ;
#17239 = CIRCLE ( 'NONE', #15736, 8.749000000000000554 ) ;
#17240 = ORIENTED_EDGE ( 'NONE', *, *, #6457, .F. ) ;
#17241 = DIRECTION ( 'NONE',  ( 1.000000000000000000, -0.000000000000000000, -0.000000000000000000 ) ) ;
#17242 = DIRECTION ( 'NONE',  ( 1.000000000000000000, -0.000000000000000000, -0.000000000000000000 ) ) ;
#17243 = CARTESIAN_POINT ( 'NONE',  ( 2.000000000000008882, 3.464101615137749945, 0.000000000000000000 ) ) ;
#17244 = VECTOR ( 'NONE', #23126, 1000.000000000000000 ) ;
#17245 = VERTEX_POINT ( 'NONE', #4903 ) ;
#17246 = CARTESIAN_POINT ( 'NONE',  ( 4.999999999999999112, -1.699438267350307008, -9.241976615262174732 ) ) ;
#17247 = VERTEX_POINT ( 'NONE', #14265 ) ;
#17248 = CARTESIAN_POINT ( 'NONE',  ( 70.75000000109247367, 8.538419263543524096, 13.53841926354352054 ) ) ;
#17249 = CARTESIAN_POINT ( 'NONE',  ( 2.828427124746191179, 2.828427124746190291, 11.62500000000001066 ) ) ;
#17250 = DIRECTION ( 'NONE',  ( 0.000000000000000000, 0.3090169943749481174, -0.9510565162951533091 ) ) ;
#17251 = EDGE_CURVE ( 'NONE', #15893, #18055, #2085, .T. ) ;
#17252 = DIRECTION ( 'NONE',  ( -0.000000000000000000, -0.000000000000000000, 1.000000000000000000 ) ) ;
#17253 = EDGE_CURVE ( 'NONE', #17055, #13420, #21525, .T. ) ;
#17254 = LINE ( 'NONE', #15467, #1051 ) ;
#17255 = CARTESIAN_POINT ( 'NONE',  ( 67.00000000109245946, 9.143825827087052716, 12.93301269999999192 ) ) ;
#17256 = ORIENTED_EDGE ( 'NONE', *, *, #972, .T. ) ;
#17257 = AXIS2_PLACEMENT_3D ( 'NONE', #13800, #2746, #10207 ) ;
#17258 = CARTESIAN_POINT ( 'NONE',  ( -1.999999999999999556, 3.464101615137754830, -3.142992957459232795 ) ) ;
#17259 = CARTESIAN_POINT ( 'NONE',  ( 1.971781867644420635E-15, -4.000000000000000000, 10.37500000273119660 ) ) ;
#17260 = EDGE_CURVE ( 'NONE', #14897, #10854, #19267, .T. ) ;
#17261 = CARTESIAN_POINT ( 'NONE',  ( 70.95000000109247651, 8.538419263543524096, 13.53841926354352054 ) ) ;
#17262 = CARTESIAN_POINT ( 'NONE',  ( 3.458734125000001214, 1.432654583217640498, 12.00000000136560452 ) ) ;
#17263 = CARTESIAN_POINT ( 'NONE',  ( 60.00000000000000711, 9.999999999999998224, 24.99999999999999645 ) ) ;
#17264 = FACE_OUTER_BOUND ( 'NONE', #3604, .T. ) ;
#17265 = ORIENTED_EDGE ( 'NONE', *, *, #18393, .T. ) ;
#17266 = CARTESIAN_POINT ( 'NONE',  ( 4.000000000000000000, 4.898587196589412829E-16, 1.800000000000001155 ) ) ;
#17267 = DIRECTION ( 'NONE',  ( 0.000000000000000000, 0.000000000000000000, -1.000000000000000000 ) ) ;
#17268 = DIRECTION ( 'NONE',  ( 1.000000000000000000, 0.000000000000000000, -0.000000000000000000 ) ) ;
#17269 = DIRECTION ( 'NONE',  ( 1.000000000000000000, 0.000000000000000000, -0.000000000000000000 ) ) ;
#17270 = VERTEX_POINT ( 'NONE', #21279 ) ;
#17271 = CARTESIAN_POINT ( 'NONE',  ( -66.65000000109247935, 7.933012699999995476, 14.99999999999999645 ) ) ;
#17272 = ORIENTED_EDGE ( 'NONE', *, *, #2644, .F. ) ;
#17273 = CARTESIAN_POINT ( 'NONE',  ( -67.15000000109247935, 11.46158073645647235, 13.53841926354352232 ) ) ;
#17274 = VERTEX_POINT ( 'NONE', #6477 ) ;
#17275 = LINE ( 'NONE', #4569, #17435 ) ;
#17276 = ORIENTED_EDGE ( 'NONE', *, *, #3064, .T. ) ;
#17277 = AXIS2_PLACEMENT_3D ( 'NONE', #3463, #14020, #17957 ) ;
#17278 = ADVANCED_FACE ( 'NONE', ( #2855 ), #3215, .T. ) ;
#17279 = ORIENTED_EDGE ( 'NONE', *, *, #7397, .F. ) ;
#17280 = CARTESIAN_POINT ( 'NONE',  ( -3.458734124999999437, 0.000000000000000000, 14.68750000136560452 ) ) ;
#17281 = CARTESIAN_POINT ( 'NONE',  ( 4.000000000000000888, 4.898587196589412829E-16, 12.62500000273119660 ) ) ;
#17282 = EDGE_CURVE ( 'NONE', #7710, #11669, #12459, .T. ) ;
#17283 = CARTESIAN_POINT ( 'NONE',  ( -68.85000000109248219, 9.999999999999998224, 17.06698730000000097 ) ) ;
#17284 = ADVANCED_FACE ( 'NONE', ( #17374 ), #21592, .F. ) ;
#17285 = CARTESIAN_POINT ( 'NONE',  ( 69.60000000109248219, 10.85617417291294551, 17.06698730000000097 ) ) ;
#17286 = CARTESIAN_POINT ( 'NONE',  ( -67.60000000109246798, 7.933012699999995476, 15.85617417291294196 ) ) ;
#17287 = DIRECTION ( 'NONE',  ( -1.000000000000000000, 0.000000000000000000, 0.000000000000000000 ) ) ;
#17288 = EDGE_CURVE ( 'NONE', #15383, #4326, #3337, .T. ) ;
#17289 = CARTESIAN_POINT ( 'NONE',  ( 58.09143183416158962, 11.31069182806491291, 12.02818770551463778 ) ) ;
#17290 = CARTESIAN_POINT ( 'NONE',  ( 45.00000000000000000, 10.00000000000001599, 34.11836509645781490 ) ) ;
#17291 = EDGE_CURVE ( 'NONE', #4502, #6195, #1061, .T. ) ;
#17292 = CARTESIAN_POINT ( 'NONE',  ( 3.458734125000000770, 4.235727675282972223E-16, 4.487500001365595459 ) ) ;
#17293 = CARTESIAN_POINT ( 'NONE',  ( 71.29999999999998295, 9.999999999999998224, 12.49999999999999289 ) ) ;
#17294 = CARTESIAN_POINT ( 'NONE',  ( 9.920644283265380691E-16, 4.000000000000000000, 13.87500000273119483 ) ) ;
#17295 = CARTESIAN_POINT ( 'NONE',  ( 72.50000000000000000, 9.999999999999998224, 17.49999999999999645 ) ) ;
#17296 = VERTEX_POINT ( 'NONE', #15595 ) ;
#17297 = CARTESIAN_POINT ( 'NONE',  ( 4.000000000000000888, 1.656854249492381248, 13.56250000000001066 ) ) ;
#17298 = ORIENTED_EDGE ( 'NONE', *, *, #4541, .F. ) ;
#17299 = CARTESIAN_POINT ( 'NONE',  ( 59.02893183416158251, 11.17458954617365663, 18.02818770551464311 ) ) ;
#17300 = SURFACE_SIDE_STYLE ('',( #8444 ) ) ;
#17301 = CARTESIAN_POINT ( 'NONE',  ( -3.458734124999999882, -1.432654583217642497, 0.8000000013655964581 ) ) ;
#17302 = CARTESIAN_POINT ( 'NONE',  ( 2.445694354108820523, -2.445694354108820079, 1.112500001365595681 ) ) ;
#17303 = VERTEX_POINT ( 'NONE', #19507 ) ;
#17304 = CARTESIAN_POINT ( 'NONE',  ( 2.435583919667260400, -11.25000000000000355, 5.000000000000079936 ) ) ;
#17305 = VERTEX_POINT ( 'NONE', #15822 ) ;
#17306 = DIRECTION ( 'NONE',  ( 1.000000000000000000, 0.000000000000000000, 0.000000000000000000 ) ) ;
#17307 = ORIENTED_EDGE ( 'NONE', *, *, #18167, .T. ) ;
#17308 = CARTESIAN_POINT ( 'NONE',  ( 57.78356816583844591, 8.689308171935074654, 12.02818770551464489 ) ) ;
#17309 = FACE_OUTER_BOUND ( 'NONE', #15484, .T. ) ;
#17310 = ADVANCED_FACE ( 'NONE', ( #13799 ), #19736, .F. ) ;
#17311 = CARTESIAN_POINT ( 'NONE',  ( 1.432654583217642053, -3.458734124999999882, -2.699999998634404541 ) ) ;
#17312 = CARTESIAN_POINT ( 'NONE',  ( -2.828427124746188515, -2.828427124746190735, 15.12500000000001066 ) ) ;
#17313 = ADVANCED_FACE ( 'NONE', ( #15931 ), #10205, .T. ) ;
#17314 = DIRECTION ( 'NONE',  ( -0.000000000000000000, -0.000000000000000000, 1.000000000000000000 ) ) ;
#17315 = CARTESIAN_POINT ( 'NONE',  ( 2.828427124746192067, -2.828427124746189847, 11.37500000000001066 ) ) ;
#17316 = CARTESIAN_POINT ( 'NONE',  ( 69.80000000109247082, 7.933012699999995476, 15.85617417291294196 ) ) ;
#17317 = EDGE_CURVE ( 'NONE', #13840, #13272, #12239, .T. ) ;
#17318 = CARTESIAN_POINT ( 'NONE',  ( -4.211140560182196957, 2.431303136016537803, -3.745885042887433514 ) ) ;
#17319 = CARTESIAN_POINT ( 'NONE',  ( 52.90856816583843880, 12.97181229448534978, 13.68930817193506755 ) ) ;
#17320 = CARTESIAN_POINT ( 'NONE',  ( 3.458734125000000770, 1.432654583217640498, 5.550000001365596347 ) ) ;
#17321 = DIRECTION ( 'NONE',  ( 0.000000000000000000, 0.000000000000000000, 1.000000000000000000 ) ) ;
#17322 = CIRCLE ( 'NONE', #4297, 4.000000000000001776 ) ;
#17323 = FILL_AREA_STYLE_COLOUR ( '', #21781 ) ;
#17324 = CARTESIAN_POINT ( 'NONE',  ( -69.45000000109247651, 9.999999999999998224, 12.93301269999999192 ) ) ;
#17325 = LINE ( 'NONE', #22240, #18479 ) ;
#17326 = DIRECTION ( 'NONE',  ( 1.000000000000000000, 0.000000000000000000, -1.224646799147353207E-16 ) ) ;
#17327 = ORIENTED_EDGE ( 'NONE', *, *, #15677, .F. ) ;
#17328 = CARTESIAN_POINT ( 'NONE',  ( 2.499999999999999556, 10.82112760146739383, -1.975651141462126059 ) ) ;
#17329 = FILL_AREA_STYLE ('',( #11957 ) ) ;
#17330 = CARTESIAN_POINT ( 'NONE',  ( -4.000000000000000000, -1.656854249492383246, 4.487500002731186655 ) ) ;
#17331 = VERTEX_POINT ( 'NONE', #3104 ) ;
#17332 = EDGE_LOOP ( 'NONE', ( #2898, #10814, #22813, #21777, #18228, #16445 ) ) ;
#17333 = PLANE ( 'NONE',  #9110 ) ;
#17334 = CARTESIAN_POINT ( 'NONE',  ( 51.93750000000000711, 10.00000000000001776, 18.99999999999999645 ) ) ;
#17335 = VERTEX_POINT ( 'NONE', #13909 ) ;
#17336 = CARTESIAN_POINT ( 'NONE',  ( -0.02448733951239248641, -4.877042772274742255, -3.751161874094027571 ) ) ;
#17337 = AXIS2_PLACEMENT_3D ( 'NONE', #9263, #20238, #3845 ) ;
#17338 = CARTESIAN_POINT ( 'NONE',  ( 68.45000000109247651, 9.999999999999998224, 12.93301269999999192 ) ) ;
#17339 = CARTESIAN_POINT ( 'NONE',  ( 68.90000000109246514, 12.06698730000000275, 15.85617417291294196 ) ) ;
#17340 = AXIS2_PLACEMENT_3D ( 'NONE', #20714, #8285, #8055 ) ;
#17341 = EDGE_CURVE ( 'NONE', #14967, #23165, #21408, .T. ) ;
#17342 = EDGE_LOOP ( 'NONE', ( #16623, #15492, #7544, #15289 ) ) ;
#17343 = DIRECTION ( 'NONE',  ( 5.546678239835225025E-32, 0.3420201433256690460, 0.9396926207859082059 ) ) ;
#17344 = CARTESIAN_POINT ( 'NONE',  ( 56.34375000000000711, 8.343145750507638070, 19.00000000000000711 ) ) ;
#17345 = CARTESIAN_POINT ( 'NONE',  ( -1.656854249492380138, -3.999999999999999112, 12.31250000273120015 ) ) ;
#17346 = CARTESIAN_POINT ( 'NONE',  ( -3.458734124999998105, -1.432654583217642275, 17.50000000136560274 ) ) ;
#17347 = CARTESIAN_POINT ( 'NONE',  ( 67.85000000218494165, 8.964466094067287116, 17.50000000000002487 ) ) ;
#17348 = FACE_OUTER_BOUND ( 'NONE', #21838, .T. ) ;
#17349 = ORIENTED_EDGE ( 'NONE', *, *, #17260, .F. ) ;
#17350 = CARTESIAN_POINT ( 'NONE',  ( -3.999999999999999112, 0.000000000000000000, 21.31370849898476649 ) ) ;
#17351 =( BOUNDED_CURVE ( )  B_SPLINE_CURVE ( 2, ( #20587, #19033, #4428, #4664, #17259, #15713, #9838, #19264, #10202 ),
 .UNSPECIFIED., .F., .F. ) 
 B_SPLINE_CURVE_WITH_KNOTS ( ( 3, 2, 2, 2, 3 ),
 ( 0.8499999999999999778, 0.8625000000000000444, 0.8750000000000000000, 0.8874999999999999556, 0.9000000000000000222 ),
 .UNSPECIFIED. ) 
 CURVE ( )  GEOMETRIC_REPRESENTATION_ITEM ( )  RATIONAL_B_SPLINE_CURVE ( ( 1.000000000000000000, 0.9238795325112867385, 1.000000000000000000, 0.9238795325112867385, 1.000000000000000000, 0.9238795325112867385, 1.000000000000000000, 0.9238795325112867385, 1.000000000000000000 ) ) 
 REPRESENTATION_ITEM ( '' )  );
#17352 = CARTESIAN_POINT ( 'NONE',  ( 0.000000000000000000, 8.152713396088806519, -3.174628368995992655 ) ) ;
#17353 = ORIENTED_EDGE ( 'NONE', *, *, #5266, .T. ) ;
#17354 = AXIS2_PLACEMENT_3D ( 'NONE', #23097, #6709, #12243 ) ;
#17355 = LINE ( 'NONE', #17114, #9018 ) ;
#17356 = DIRECTION ( 'NONE',  ( 0.000000000000000000, -0.000000000000000000, 1.000000000000000000 ) ) ;
#17357 = DIRECTION ( 'NONE',  ( -1.000000000000000000, 0.000000000000000000, 0.000000000000000000 ) ) ;
#17358 = AXIS2_PLACEMENT_3D ( 'NONE', #20207, #22002, #14741 ) ;
#17359 = CARTESIAN_POINT ( 'NONE',  ( -60.00000000000000711, 15.00000000000000000, 20.00000000000001421 ) ) ;
#17360 = EDGE_LOOP ( 'NONE', ( #12865, #15824 ) ) ;
#17361 = CARTESIAN_POINT ( 'NONE',  ( 6.500000000000000000, 3.752776749732573247, -3.119443416399232394 ) ) ;
#17362 = ORIENTED_EDGE ( 'NONE', *, *, #3688, .F. ) ;
#17363 = CARTESIAN_POINT ( 'NONE',  ( -65.00000000000000000, 9.999999999999998224, 14.99999999999999645 ) ) ;
#17364 = CARTESIAN_POINT ( 'NONE',  ( 71.20000000218495018, 7.499999999999996447, 14.99999999999999645 ) ) ;
#17365 = DIRECTION ( 'NONE',  ( 1.000000000000000000, 0.000000000000000000, 0.000000000000000000 ) ) ;
#17366 = DIRECTION ( 'NONE',  ( 1.000000000000000000, 7.703719777548943412E-32, 0.000000000000000000 ) ) ;
#17367 = CARTESIAN_POINT ( 'NONE',  ( 69.05000000109247082, 9.999999999999998224, 17.06698730000000097 ) ) ;
#17368 = ORIENTED_EDGE ( 'NONE', *, *, #6402, .F. ) ;
#17369 = PLANE ( 'NONE',  #3402 ) ;
#17370 = CARTESIAN_POINT ( 'NONE',  ( 35.00000000000000000, 7.500000000000001776, -20.00000000000000355 ) ) ;
#17371 = CARTESIAN_POINT ( 'NONE',  ( 70.85000000109246798, 7.933012699999995476, 14.99999999999999645 ) ) ;
#17372 = CARTESIAN_POINT ( 'NONE',  ( 1.025207404391860050E-15, 3.458734125000000326, 15.18750000136560452 ) ) ;
#17373 = B_SPLINE_CURVE_WITH_KNOTS ( 'NONE', 3,
 ( #10379, #16106, #113, #15763 ),
 .UNSPECIFIED., .F., .F.,
 ( 4, 4 ),
 ( 8.673617379884032583E-19, 0.001664000150434504811 ),
 .UNSPECIFIED. ) ;
#17374 = FACE_OUTER_BOUND ( 'NONE', #14029, .T. ) ;
#17375 = CARTESIAN_POINT ( 'NONE',  ( 14.99999999999999289, 10.00000000000000000, -50.00000000000000000 ) ) ;
#17376 = EDGE_LOOP ( 'NONE', ( #23488, #18884, #20418 ) ) ;
#17377 = CARTESIAN_POINT ( 'NONE',  ( -4.000000000000000888, 1.656854249492380804, -2.762499999999997069 ) ) ;
#17378 = CARTESIAN_POINT ( 'NONE',  ( 1.799999999999996048, 0.000000000000000000, -6.000000000000022204 ) ) ;
#17379 = CARTESIAN_POINT ( 'NONE',  ( 0.000000000000000000, -1.239665997526817165, -9.314797388894906049 ) ) ;
#17380 = LINE ( 'NONE', #951, #2690 ) ;
#17381 = PRODUCT_DEFINITION_SHAPE ( 'NONE', 'NONE',  #20705 ) ;
#17382 = ORIENTED_EDGE ( 'NONE', *, *, #14674, .T. ) ;
#17383 = ADVANCED_FACE ( 'NONE', ( #14142 ), #4770, .T. ) ;
#17384 = DIRECTION ( 'NONE',  ( 1.224646799147353207E-16, -0.000000000000000000, 1.000000000000000000 ) ) ;
#17385 = ORIENTED_EDGE ( 'NONE', *, *, #11094, .T. ) ;
#17386 = CARTESIAN_POINT ( 'NONE',  ( -66.55000000109247082, 11.46158073645647235, 16.46158073645647235 ) ) ;
#17387 = ITEM_DEFINED_TRANSFORMATION ( 'NONE', 'NONE', #13011,  #7318 ) ;
#17388 = VERTEX_POINT ( 'NONE', #10562 ) ;
#17389 = CARTESIAN_POINT ( 'NONE',  ( 0.000000000000000000, 0.000000000000000000, -4.974599999999998801 ) ) ;
#17390 = VERTEX_POINT ( 'NONE', #17837 ) ;
#17391 = ORIENTED_EDGE ( 'NONE', *, *, #16256, .F. ) ;
#17392 = CARTESIAN_POINT ( 'NONE',  ( -1.432654583217639832, -3.458734125000000326, 11.87500000136560452 ) ) ;
#17393 = AXIS2_PLACEMENT_3D ( 'NONE', #8192, #15506, #22774 ) ;
#17394 = EDGE_CURVE ( 'NONE', #15383, #17500, #19858, .T. ) ;
#17395 = CARTESIAN_POINT ( 'NONE',  ( 51.93750000000000711, 10.00000000000000711, 17.99999999999999645 ) ) ;
#17396 = CARTESIAN_POINT ( 'NONE',  ( -65.80000000109247082, 7.933012699999995476, 15.85617417291294196 ) ) ;
#17397 = AXIS2_PLACEMENT_3D ( 'NONE', #15568, #8011, #17231 ) ;
#17398 = CARTESIAN_POINT ( 'NONE',  ( 66.65000000109247935, 7.933012699999995476, 14.99999999999999645 ) ) ;
#17399 = VECTOR ( 'NONE', #17652, 1000.000000000000000 ) ;
#17400 = CARTESIAN_POINT ( 'NONE',  ( -71.34999999999999432, 11.03553390593273598, 12.49999999999999289 ) ) ;
#17401 = VECTOR ( 'NONE', #16052, 1000.000000000000000 ) ;
#17402 = CARTESIAN_POINT ( 'NONE',  ( -71.59999999999999432, 11.76776695296636888, 16.76776695296636532 ) ) ;
#17403 = CARTESIAN_POINT ( 'NONE',  ( 53.40393183416157541, 13.02818770551463778, 13.82541045382633982 ) ) ;
#17404 = CARTESIAN_POINT ( 'NONE',  ( 2.100000000000000089, 0.000000000000000000, -4.694516984716113228 ) ) ;
#17405 = CARTESIAN_POINT ( 'NONE',  ( -2.445694354108819635, -2.445694354108820967, 5.112500001365595459 ) ) ;
#17406 = DIRECTION ( 'NONE',  ( -0.8191520442889902442, 0.000000000000000000, -0.5735764363510482688 ) ) ;
#17407 = CARTESIAN_POINT ( 'NONE',  ( -3.999999999999999112, 1.656854249492380804, 13.06250000273119660 ) ) ;
#17408 = LINE ( 'NONE', #8306, #20255 ) ;
#17409 = ORIENTED_EDGE ( 'NONE', *, *, #9390, .F. ) ;
#17410 = EDGE_CURVE ( 'NONE', #4211, #6665, #20201, .T. ) ;
#17411 = PLANE ( 'NONE',  #22341 ) ;
#17412 = ORIENTED_EDGE ( 'NONE', *, *, #23195, .T. ) ;
#17413 = CARTESIAN_POINT ( 'NONE',  ( 58.74768183416157541, 7.123453452023678523, 17.78030770151605822 ) ) ;
#17414 = DIRECTION ( 'NONE',  ( 0.000000000000000000, 0.000000000000000000, 1.000000000000000000 ) ) ;
#17415 = CARTESIAN_POINT ( 'NONE',  ( 2.445694354108820079, 2.445694354108820523, 2.362500001365596791 ) ) ;
#17416 = EDGE_CURVE ( 'NONE', #20854, #11744, #541, .T. ) ;
#17417 = CARTESIAN_POINT ( 'NONE',  ( -3.458734124999999882, -1.432654583217642275, -1.199999998634403209 ) ) ;
#17418 = ORIENTED_EDGE ( 'NONE', *, *, #18855, .T. ) ;
#17419 = TOROIDAL_SURFACE ( 'NONE', #7088, 8.800000000000023803, 0.2000000000000000944 ) ;
#17420 = CYLINDRICAL_SURFACE ( 'NONE', #22881, 4.000000000000000000 ) ;
#17421 = AXIS2_PLACEMENT_3D ( 'NONE', #339, #16298, #18428 ) ;
#17422 = VERTEX_POINT ( 'NONE', #16287 ) ;
#17423 = CYLINDRICAL_SURFACE ( 'NONE', #7225, 6.735000000000022524 ) ;
#17424 = ORIENTED_EDGE ( 'NONE', *, *, #9861, .F. ) ;
#17425 = EDGE_CURVE ( 'NONE', #10489, #844, #6123, .T. ) ;
#17426 = CARTESIAN_POINT ( 'NONE',  ( 57.12731816583843170, 12.16943976678978601, 17.07320092032949432 ) ) ;
#17427 = EDGE_CURVE ( 'NONE', #7757, #23046, #3462, .T. ) ;
#17428 = CARTESIAN_POINT ( 'NONE',  ( -68.60000000218495586, 9.999999999999998224, 17.49999999999999645 ) ) ;
#17429 = CARTESIAN_POINT ( 'NONE',  ( -2.445694354108820523, 2.445694354108820523, -2.137499998634403653 ) ) ;
#17430 = CARTESIAN_POINT ( 'NONE',  ( -71.29999999999998295, 9.999999999999998224, 12.49999999999999289 ) ) ;
#17431 = CARTESIAN_POINT ( 'NONE',  ( -1.432654583217639166, 3.458734125000000770, 18.50000000136560629 ) ) ;
#17432 = CARTESIAN_POINT ( 'NONE',  ( 4.000000000000001776, -1.656854249492379694, 14.56250000273119660 ) ) ;
#17433 = CARTESIAN_POINT ( 'NONE',  ( -72.09999999999999432, 9.999999999999998224, 12.49999999999999289 ) ) ;
#17434 = CARTESIAN_POINT ( 'NONE',  ( 70.55000000109247082, 8.538419263543522320, 16.46158073645647235 ) ) ;
#17436 = DIRECTION ( 'NONE',  ( 0.000000000000000000, 0.000000000000000000, 1.000000000000000000 ) ) ;
#17435 = VECTOR ( 'NONE', #8291, 1000.000000000000114 ) ;
#17437 = CARTESIAN_POINT ( 'NONE',  ( 54.59606816583844591, 11.17458954617364242, 11.97181229448534800 ) ) ;
#17438 = EDGE_CURVE ( 'NONE', #23070, #14683, #4537, .T. ) ;
#17439 = AXIS2_PLACEMENT_3D ( 'NONE', #2945, #680, #806 ) ;
#17440 = CARTESIAN_POINT ( 'NONE',  ( -3.458734125000000770, 1.432654583217640498, 0.9250000013655964581 ) ) ;
#17441 = CARTESIAN_POINT ( 'NONE',  ( 0.6666666666666658525, -4.233901974057276085, -3.300726591567086476 ) ) ;
#17442 = DIRECTION ( 'NONE',  ( -1.224646799147353454E-16, 0.000000000000000000, -1.000000000000000000 ) ) ;
#17443 = CARTESIAN_POINT ( 'NONE',  ( -69.15000000109246514, 8.538419263543522320, 16.46158073645647235 ) ) ;
#17444 = DIRECTION ( 'NONE',  ( 0.000000000000000000, -1.000000000000000000, 0.000000000000000000 ) ) ;
#17445 = CARTESIAN_POINT ( 'NONE',  ( 4.999999999999999112, -5.538577986808947529, 6.772677083992368452 ) ) ;
#17446 = VERTEX_POINT ( 'NONE', #21995 ) ;
#17447 = CARTESIAN_POINT ( 'NONE',  ( 59.71875000000000711, 13.00000000000000711, 16.24264068711927322 ) ) ;
#17448 = SURFACE_STYLE_USAGE ( .BOTH. , #10155 ) ;
#17449 = CARTESIAN_POINT ( 'NONE',  ( -2.828427124746189403, -2.828427124746190735, 4.550000002731186655 ) ) ;
#17450 = ADVANCED_FACE ( 'NONE', ( #5489 ), #10680, .T. ) ;
#17451 = ORIENTED_EDGE ( 'NONE', *, *, #3835, .F. ) ;
#17452 = CIRCLE ( 'NONE', #7117, 8.749000000000004107 ) ;
#17453 = ORIENTED_EDGE ( 'NONE', *, *, #3784, .T. ) ;
#17454 = VECTOR ( 'NONE', #10538, 1000.000000000000000 ) ;
#17455 = DIRECTION ( 'NONE',  ( 0.3420201433256622181, 0.9396926207859107594, -6.162975822039141593E-32 ) ) ;
#17456 = CARTESIAN_POINT ( 'NONE',  ( -66.49999999999998579, 9.999999999999998224, 12.49999999999999289 ) ) ;
#17457 = EDGE_LOOP ( 'NONE', ( #10282, #16303, #12574, #4302 ) ) ;
#17458 = EDGE_CURVE ( 'NONE', #2919, #12703, #9231, .T. ) ;
#17459 = CARTESIAN_POINT ( 'NONE',  ( 1.390230914382191596, 4.043987460488659202, -3.502507215260488582 ) ) ;
#17460 = EDGE_CURVE ( 'NONE', #20225, #19081, #20108, .T. ) ;
#17461 = CARTESIAN_POINT ( 'NONE',  ( 67.25000000109247367, 9.999999999999998224, 17.06698730000000097 ) ) ;
#17462 = CARTESIAN_POINT ( 'NONE',  ( 67.90000000109245093, 10.85617417291294551, 12.93301269999999370 ) ) ;
#17463 = ORIENTED_EDGE ( 'NONE', *, *, #20093, .T. ) ;
#17464 = PLANE ( 'NONE',  #9570 ) ;
#17465 = CARTESIAN_POINT ( 'NONE',  ( 58.31250000000000000, 14.00000000000000000, 14.99999999999997691 ) ) ;
#17466 = CARTESIAN_POINT ( 'NONE',  ( 3.458734125000000326, 1.432654583217640498, 5.300000001365596347 ) ) ;
#17467 = LINE ( 'NONE', #13764, #3994 ) ;
#17468 = DIRECTION ( 'NONE',  ( -1.000000000000000000, -0.000000000000000000, 0.000000000000000000 ) ) ;
#17469 = DIRECTION ( 'NONE',  ( 1.000000000000000000, 0.000000000000000000, 0.000000000000000000 ) ) ;
#17470 = EDGE_LOOP ( 'NONE', ( #10362, #13621, #21647 ) ) ;
#17471 = CARTESIAN_POINT ( 'NONE',  ( -67.40000000218495302, 9.999999999999998224, 12.49999999999999289 ) ) ;
#17472 = CARTESIAN_POINT ( 'NONE',  ( -19.99999999999999645, -9.000000000000003553, 5.000000000000079936 ) ) ;
#17473 = CARTESIAN_POINT ( 'NONE',  ( 60.00000000000000711, -9.999999999999998224, 24.99999999999999645 ) ) ;
#17474 = ORIENTED_EDGE ( 'NONE', *, *, #972, .F. ) ;
#17475 = DIRECTION ( 'NONE',  ( -1.224646799147353207E-16, 0.000000000000000000, -1.000000000000000000 ) ) ;
#17476 = DIRECTION ( 'NONE',  ( 0.000000000000000000, 0.000000000000000000, 1.000000000000000000 ) ) ;
#17477 = ADVANCED_FACE ( 'NONE', ( #12824 ), #20082, .F. ) ;
#17478 = DIRECTION ( 'NONE',  ( -1.000000000000000000, 0.000000000000000000, 0.000000000000000000 ) ) ;
#17479 = ORIENTED_EDGE ( 'NONE', *, *, #18128, .T. ) ;
#17480 = DIRECTION ( 'NONE',  ( -1.224646799147353207E-16, 0.000000000000000000, -1.000000000000000000 ) ) ;
#17481 = ORIENTED_EDGE ( 'NONE', *, *, #8400, .T. ) ;
#17482 = EDGE_CURVE ( 'NONE', #20225, #14363, #5539, .T. ) ;
#17483 = CARTESIAN_POINT ( 'NONE',  ( 71.50000000109248788, 7.933012699999995476, 14.14382582708705094 ) ) ;
#17484 = CARTESIAN_POINT ( 'NONE',  ( 69.90000000218495302, 11.76776695296636888, 13.23223304703362579 ) ) ;
#17485 = CARTESIAN_POINT ( 'NONE',  ( 4.999999999999999112, 7.958834565716766285, 7.593217523260607393 ) ) ;
#17486 = DIRECTION ( 'NONE',  ( 0.000000000000000000, 0.000000000000000000, -1.000000000000000000 ) ) ;
#17487 = CARTESIAN_POINT ( 'NONE',  ( 67.40000000109247935, 10.85617417291294551, 17.06698730000000097 ) ) ;
#17488 = VERTEX_POINT ( 'NONE', #207 ) ;
#17489 = FACE_OUTER_BOUND ( 'NONE', #5950, .T. ) ;
#17490 = FACE_OUTER_BOUND ( 'NONE', #10400, .T. ) ;
#17491 = CARTESIAN_POINT ( 'NONE',  ( 68.35000000109246798, 8.538419263543522320, 16.46158073645647235 ) ) ;
#17492 = CARTESIAN_POINT ( 'NONE',  ( 3.458734125000002546, -1.432654583217639610, 17.12500000136560629 ) ) ;
#17493 = CARTESIAN_POINT ( 'NONE',  ( -0.3649867057748643617, 3.983313282257324950, 10.00000000000000888 ) ) ;
#17494 = AXIS2_PLACEMENT_3D ( 'NONE', #1726, #9192, #18258 ) ;
#17495 = CARTESIAN_POINT ( 'NONE',  ( -65.00000000000000000, -10.00000000000000178, 14.99999999999999467 ) ) ;
#17496 = ORIENTED_EDGE ( 'NONE', *, *, #7139, .F. ) ;
#17497 = CARTESIAN_POINT ( 'NONE',  ( -2.449293598294706907E-16, 4.000000000000000000, -2.949999999999997957 ) ) ;
#17498 = CARTESIAN_POINT ( 'NONE',  ( 23.53786173033275375, -11.25000000000000355, 10.00000000000008882 ) ) ;
#17499 = CARTESIAN_POINT ( 'NONE',  ( 2.500000000000000000, 1.178949249685212974, -2.042000000000001148 ) ) ;
#17500 = VERTEX_POINT ( 'NONE', #11738 ) ;
#17501 = CARTESIAN_POINT ( 'NONE',  ( 0.000000000000000000, -1.464956435139620927, 10.90201369670498366 ) ) ;
#17502 = VERTEX_POINT ( 'NONE', #18654 ) ;
#17503 = AXIS2_PLACEMENT_3D ( 'NONE', #7605, #12883, #14928 ) ;
#17504 = CARTESIAN_POINT ( 'NONE',  ( -69.00000000109245946, 10.85617417291294551, 17.06698729999999742 ) ) ;
#17505 = CONTEXT_DEPENDENT_SHAPE_REPRESENTATION ( #16510, #9731 ) ;
#17506 = ORIENTED_EDGE ( 'NONE', *, *, #14362, .F. ) ;
#17507 = LINE ( 'NONE', #2642, #4801 ) ;
#17508 = ORIENTED_EDGE ( 'NONE', *, *, #10074, .T. ) ;
#17509 = PRESENTATION_LAYER_ASSIGNMENT (  '', '', ( #2178 ) ) ;
#17510 = ORIENTED_EDGE ( 'NONE', *, *, #14245, .T. ) ;
#17511 = CARTESIAN_POINT ( 'NONE',  ( -2.445694354108819191, 2.445694354108820523, 12.56250000136560629 ) ) ;
#17512 = DIRECTION ( 'NONE',  ( -1.000000000000000000, -0.000000000000000000, 0.000000000000000000 ) ) ;
#17513 = AXIS2_PLACEMENT_3D ( 'NONE', #14247, #14361, #21745 ) ;
#17514 = DIRECTION ( 'NONE',  ( 0.000000000000000000, -0.9510565162951499785, -0.3090169943749581649 ) ) ;
#17515 = PLANE ( 'NONE',  #4137 ) ;
#17516 = EDGE_CURVE ( 'NONE', #17488, #19299, #4400, .T. ) ;
#17517 = CARTESIAN_POINT ( 'NONE',  ( -70.79999999999999716, 11.76776695296636888, 16.76776695296636532 ) ) ;
#17518 = CARTESIAN_POINT ( 'NONE',  ( -71.29999999999998295, 9.999999999999998224, 12.49999999999999289 ) ) ;
#17519 = CARTESIAN_POINT ( 'NONE',  ( 53.31018183416157541, 12.99999999999999822, 15.06805114094562192 ) ) ;
#17520 = DIRECTION ( 'NONE',  ( 0.000000000000000000, 0.4999999999999990008, -0.8660254037844391517 ) ) ;
#17521 = VECTOR ( 'NONE', #7305, 1000.000000000000000 ) ;
#17522 = CARTESIAN_POINT ( 'NONE',  ( -1.432654583217641164, -3.458734125000000326, -0.8249999986344030978 ) ) ;
#17523 = CARTESIAN_POINT ( 'NONE',  ( 4.000000000000001776, -1.656854249492379694, 13.43750000000001243 ) ) ;
#17524 = FACE_OUTER_BOUND ( 'NONE', #13034, .T. ) ;
#17525 = CARTESIAN_POINT ( 'NONE',  ( -1.656854249492379250, 4.000000000000000000, 13.93750000273119483 ) ) ;
#17526 = CARTESIAN_POINT ( 'NONE',  ( -68.60000000218495586, 9.999999999999998224, 17.49999999999999645 ) ) ;
#17527 = AXIS2_PLACEMENT_3D ( 'NONE', #4118, #6041, #2434 ) ;
#17528 = ORIENTED_EDGE ( 'NONE', *, *, #3933, .F. ) ;
#17529 = AXIS2_PLACEMENT_3D ( 'NONE', #2072, #10976, #22190 ) ;
#17530 = CARTESIAN_POINT ( 'NONE',  ( -2.828427124746189403, 2.828427124746190291, 13.87500000000001066 ) ) ;
#17531 = ORIENTED_EDGE ( 'NONE', *, *, #12425, .F. ) ;
#17532 = CARTESIAN_POINT ( 'NONE',  ( 53.96643183416157541, 7.028187705514638672, 13.68930817193508531 ) ) ;
#17533 = CARTESIAN_POINT ( 'NONE',  ( 2.445694354108820523, -2.445694354108820079, 0.1125000013655966247 ) ) ;
#17534 = EDGE_LOOP ( 'NONE', ( #17909, #322, #5771, #22645 ) ) ;
#17535 = FACE_OUTER_BOUND ( 'NONE', #5952, .T. ) ;
#17536 = VERTEX_POINT ( 'NONE', #22236 ) ;
#17537 = DIRECTION ( 'NONE',  ( 0.000000000000000000, 0.000000000000000000, -1.000000000000000000 ) ) ;
#17538 = ORIENTED_EDGE ( 'NONE', *, *, #8863, .F. ) ;
#17539 = CARTESIAN_POINT ( 'NONE',  ( 56.56481816583843170, 6.999999999999998224, 15.06805114094563436 ) ) ;
#17540 = AXIS2_PLACEMENT_3D ( 'NONE', #14167, #5043, #12375 ) ;
#17541 = CARTESIAN_POINT ( 'NONE',  ( -66.40000000218495302, 7.499999999999996447, 14.99999999999999645 ) ) ;
#17542 = CARTESIAN_POINT ( 'NONE',  ( -4.736472119667250347, -11.25000000000000355, 10.00000000000008882 ) ) ;
#17543 = AXIS2_PLACEMENT_3D ( 'NONE', #23260, #10488, #2789 ) ;
#17544 = EDGE_CURVE ( 'NONE', #21867, #4634, #563, .T. ) ;
#17545 = AXIS2_PLACEMENT_3D ( 'NONE', #5617, #17000, #12949 ) ;
#17546 = CARTESIAN_POINT ( 'NONE',  ( 0.000000000000000000, 0.000000000000000000, 0.000000000000000000 ) ) ;
#17547 = COLOUR_RGB ( '', 0.31764706, 0.68627451, 0.89019608) ;
#17548 = CARTESIAN_POINT ( 'NONE',  ( 3.458734125000002546, -1.432654583217639610, 18.12500000136560274 ) ) ;
#17549 = ADVANCED_FACE ( 'NONE', ( #13171 ), #13525, .T. ) ;
#17550 = CARTESIAN_POINT ( 'NONE',  ( 4.000000000000001776, -1.656854249492379694, 13.56250000273119660 ) ) ;
#17551 = CARTESIAN_POINT ( 'NONE',  ( 60.00000000000000711, 12.12132034355963484, 12.87867965644034740 ) ) ;
#17552 = CARTESIAN_POINT ( 'NONE',  ( 68.75000000109247367, 11.46158073645647235, 16.46158073645647235 ) ) ;
#17553 = LINE ( 'NONE', #2802, #21790 ) ;
#17554 = CARTESIAN_POINT ( 'NONE',  ( 50.28356816583843880, 8.689308171935074654, 12.02818770551464489 ) ) ;
#17555 = CARTESIAN_POINT ( 'NONE',  ( -2.117863837641485618E-16, 3.458734125000000770, -0.2624999986344037084 ) ) ;
#17556 = CARTESIAN_POINT ( 'NONE',  ( 1.999999999999998224, -3.464101615137772594, -3.142992957459239012 ) ) ;
#17557 = ADVANCED_FACE ( 'NONE', ( #9695 ), #16991, .T. ) ;
#17558 = CARTESIAN_POINT ( 'NONE',  ( -69.90000000109246514, 9.143825827087049163, 17.06698730000000097 ) ) ;
#17559 = AXIS2_PLACEMENT_3D ( 'NONE', #9964, #707, #2143 ) ;
#17560 = ORIENTED_EDGE ( 'NONE', *, *, #9539, .F. ) ;
#17561 = DIRECTION ( 'NONE',  ( 0.000000000000000000, 0.000000000000000000, -1.000000000000000000 ) ) ;
#17562 = ORIENTED_EDGE ( 'NONE', *, *, #16652, .F. ) ;
#17563 = CARTESIAN_POINT ( 'NONE',  ( 2.828427124746192067, -2.828427124746189847, 15.50000000273119660 ) ) ;
#17564 = PRESENTATION_STYLE_ASSIGNMENT (( #21005 ) ) ;
#17565 = CARTESIAN_POINT ( 'NONE',  ( -4.000000000000000000, -1.656854249492383246, 0.4875000027311865436 ) ) ;
#17566 = EDGE_LOOP ( 'NONE', ( #9658, #498, #16402, #22359 ) ) ;
#17567 = ORIENTED_EDGE ( 'NONE', *, *, #2796, .F. ) ;
#17568 = CARTESIAN_POINT ( 'NONE',  ( -1.654252653721913102, -3.663718938583024443, -0.01223254789874440342 ) ) ;
#17569 = VECTOR ( 'NONE', #5361, 1000.000000000000000 ) ;
#17570 = CARTESIAN_POINT ( 'NONE',  ( 118.3095189484530181, 10.00000000000001599, 15.00000000000003020 ) ) ;
#17571 = ORIENTED_EDGE ( 'NONE', *, *, #15642, .F. ) ;
#17572 = CARTESIAN_POINT ( 'NONE',  ( -0.02511973781850462134, 4.877415612947412882, -3.751298745799839462 ) ) ;
#17573 = AXIS2_PLACEMENT_3D ( 'NONE', #10676, #2971, #5249 ) ;
#17574 = CARTESIAN_POINT ( 'NONE',  ( 69.35000000109248219, 11.46158073645647235, 13.53841926354352232 ) ) ;
#17575 = VECTOR ( 'NONE', #5130, 1000.000000000000000 ) ;
#17576 = CARTESIAN_POINT ( 'NONE',  ( 66.60000000109246798, 10.85617417291294551, 17.06698729999999742 ) ) ;
#17577 = ADVANCED_FACE ( 'NONE', ( #15096 ), #22351, .T. ) ;
#17578 = PRODUCT_DEFINITION_FORMATION_WITH_SPECIFIED_SOURCE ( 'ANY', '', #16983, .NOT_KNOWN. ) ;
#17579 = VECTOR ( 'NONE', #10806, 1000.000000000000000 ) ;
#17580 = DIRECTION ( 'NONE',  ( 1.000000000000000000, 0.000000000000000000, 0.000000000000000000 ) ) ;
#17581 = CIRCLE ( 'NONE', #20986, 4.999999999999999112 ) ;
#17582 = CARTESIAN_POINT ( 'NONE',  ( 53.25000000000000711, 7.171572875253819923, 17.82842712474619873 ) ) ;
#17583 = CARTESIAN_POINT ( 'NONE',  ( 3.458734125000000326, 4.235727675282971730E-16, 5.237500001365596347 ) ) ;
#17584 = EDGE_CURVE ( 'NONE', #22779, #17107, #4286, .T. ) ;
#17585 = CARTESIAN_POINT ( 'NONE',  ( 1.025207404391860050E-15, 3.458734125000000326, 16.18750000136560629 ) ) ;
#17586 = LINE ( 'NONE', #10057, #18176 ) ;
#17587 = EDGE_CURVE ( 'NONE', #1712, #5741, #4046, .T. ) ;
#17588 = LINE ( 'NONE', #22605, #12868 ) ;
#17589 = VERTEX_POINT ( 'NONE', #13642 ) ;
#17590 = CARTESIAN_POINT ( 'NONE',  ( -20.00005080000000035, 0.000000000000000000, 0.000000000000000000 ) ) ;
#17591 = CARTESIAN_POINT ( 'NONE',  ( 25.00005080000000035, 0.000000000000000000, 1.000000000000000000 ) ) ;
#17592 = DIRECTION ( 'NONE',  ( -1.000000000000000000, -0.000000000000000000, 0.000000000000000000 ) ) ;
#17593 = CIRCLE ( 'NONE', #1886, 0.03079999999999836341 ) ;
#17594 = ORIENTED_EDGE ( 'NONE', *, *, #20475, .F. ) ;
#17595 = AXIS2_PLACEMENT_3D ( 'NONE', #20287, #420, #7747 ) ;
#17596 = CARTESIAN_POINT ( 'NONE',  ( 0.3461262719736147297, -4.658553426539303821, -3.671615880910379381 ) ) ;
#17597 = DIRECTION ( 'NONE',  ( -1.000000000000000000, 0.000000000000000000, 0.000000000000000000 ) ) ;
#17598 = DIRECTION ( 'NONE',  ( -1.000000000000000000, 0.000000000000000000, 0.000000000000000000 ) ) ;
#17599 = VERTEX_POINT ( 'NONE', #3918 ) ;
#17600 = CARTESIAN_POINT ( 'NONE',  ( 66.05000000218494449, 12.50000000000000000, 16.03553390593273775 ) ) ;
#17601 = VERTEX_POINT ( 'NONE', #2117 ) ;
#17602 = CARTESIAN_POINT ( 'NONE',  ( -1.656854249492379472, 4.000000000000000000, 17.81250000000001066 ) ) ;
#17603 = AXIS2_PLACEMENT_3D ( 'NONE', #6542, #2694, #21113 ) ;
#17604 = CARTESIAN_POINT ( 'NONE',  ( 69.85000000218495586, 11.03553390593273598, 12.49999999999999289 ) ) ;
#17605 = CARTESIAN_POINT ( 'NONE',  ( 2.828427124746192067, -2.828427124746189847, 19.37500000000001066 ) ) ;
#17606 = DIRECTION ( 'NONE',  ( 0.000000000000000000, 0.5877852522924688072, 0.8090169943749507819 ) ) ;
#17607 = CARTESIAN_POINT ( 'NONE',  ( 66.05000000109247082, 7.933012699999995476, 14.99999999999999645 ) ) ;
#17608 = ORIENTED_EDGE ( 'NONE', *, *, #16857, .F. ) ;
#17609 = CIRCLE ( 'NONE', #17976, 4.000000000000002665 ) ;
#17610 = CARTESIAN_POINT ( 'NONE',  ( -65.00000000000000000, -15.00000000000000000, 10.00000000000008882 ) ) ;
#17611 = EDGE_CURVE ( 'NONE', #6374, #17685, #7888, .T. ) ;
#17612 = FACE_OUTER_BOUND ( 'NONE', #8879, .T. ) ;
#17613 = EDGE_CURVE ( 'NONE', #9536, #8981, #13227, .T. ) ;
#17614 = CARTESIAN_POINT ( 'NONE',  ( 69.45000000109247651, 9.999999999999998224, 12.93301269999999192 ) ) ;
#17615 = CARTESIAN_POINT ( 'NONE',  ( 2.445694354108821411, 2.445694354108820523, 11.06250000136560452 ) ) ;
#17616 = VECTOR ( 'NONE', #19132, 1000.000000000000000 ) ;
#17617 = DIRECTION ( 'NONE',  ( -1.000000000000000000, 0.000000000000000000, 0.000000000000000000 ) ) ;
#17618 = ADVANCED_FACE ( 'NONE', ( #20557 ), #8012, .F. ) ;
#17619 = B_SPLINE_CURVE_WITH_KNOTS ( 'NONE', 3,
 ( #9281, #16567, #146, #7478 ),
 .UNSPECIFIED., .F., .F.,
 ( 4, 4 ),
 ( 0.000000000000000000, 0.002452478801916376308 ),
 .UNSPECIFIED. ) ;
#17620 = CARTESIAN_POINT ( 'NONE',  ( 4.999999999999999112, 1.239665997527020558, -9.314797388894877628 ) ) ;
#17621 = AXIS2_PLACEMENT_3D ( 'NONE', #18569, #2152, #11417 ) ;
#17622 = EDGE_LOOP ( 'NONE', ( #4088, #22777, #14145, #10633 ) ) ;
#17623 = CARTESIAN_POINT ( 'NONE',  ( -4.000000000000000000, -1.656854249492383246, -2.637499999999998845 ) ) ;
#17624 = DIRECTION ( 'NONE',  ( 1.000000000000000000, -0.000000000000000000, -0.000000000000000000 ) ) ;
#17625 = CARTESIAN_POINT ( 'NONE',  ( -2.828427124746189403, -2.828427124746190735, 0.5500000027311869877 ) ) ;
#17626 = LINE ( 'NONE', #10333, #22185 ) ;
#17627 = ORIENTED_EDGE ( 'NONE', *, *, #12783, .T. ) ;
#17628 = CARTESIAN_POINT ( 'NONE',  ( -2.828427124746188515, -2.828427124746190735, 13.25000000273119660 ) ) ;
#17629 = ORIENTED_EDGE ( 'NONE', *, *, #3302, .T. ) ;
#17630 = DIRECTION ( 'NONE',  ( -0.000000000000000000, 0.000000000000000000, -1.000000000000000000 ) ) ;
#17631 = ORIENTED_EDGE ( 'NONE', *, *, #10991, .T. ) ;
#17632 = CARTESIAN_POINT ( 'NONE',  ( -19.99999999999999645, -9.000000000000003553, 5.000000000000079936 ) ) ;
#17633 = VERTEX_POINT ( 'NONE', #19001 ) ;
#17634 = ORIENTED_EDGE ( 'NONE', *, *, #6263, .T. ) ;
#17635 = CARTESIAN_POINT ( 'NONE',  ( 3.458734125000001658, 1.432654583217640498, 11.25000000136560452 ) ) ;
#17636 = DIRECTION ( 'NONE',  ( 1.000000000000000000, 0.000000000000000000, 0.000000000000000000 ) ) ;
#17637 = CIRCLE ( 'NONE', #2687, 8.749000000000002331 ) ;
#17638 = DIRECTION ( 'NONE',  ( -1.000000000000000000, -0.000000000000000000, 0.000000000000000000 ) ) ;
#17639 = STYLED_ITEM ( 'NONE', ( #23349 ), #5892 ) ;
#17640 = CARTESIAN_POINT ( 'NONE',  ( 66.10000000109248219, 10.85617417291294551, 12.93301269999999192 ) ) ;
#17641 = CARTESIAN_POINT ( 'NONE',  ( -69.09999999999999432, 12.50000000000000000, 14.99999999999999645 ) ) ;
#17642 = EDGE_CURVE ( 'NONE', #10312, #476, #13986, .T. ) ;
#17643 = DIRECTION ( 'NONE',  ( 0.000000000000000000, 0.000000000000000000, -1.000000000000000000 ) ) ;
#17644 = CARTESIAN_POINT ( 'NONE',  ( 60.00000000000001421, 13.96345569325843172, 15.23269126663819506 ) ) ;
#17645 = CARTESIAN_POINT ( 'NONE',  ( -2.445694354108820523, 2.445694354108820523, 0.8625000013655955700 ) ) ;
#17646 = FACE_OUTER_BOUND ( 'NONE', #20809, .T. ) ;
#17647 = CARTESIAN_POINT ( 'NONE',  ( 50.00000000000000000, 10.00000000000001599, 17.50000000000003197 ) ) ;
#17648 = CARTESIAN_POINT ( 'NONE',  ( -3.458734124999998993, 1.432654583217640276, 19.37500000136560274 ) ) ;
#17649 = DIRECTION ( 'NONE',  ( -1.000000000000000000, 0.000000000000000000, -0.000000000000000000 ) ) ;
#17650 = AXIS2_PLACEMENT_3D ( 'NONE', #2473, #18999, #22828 ) ;
#17651 = EDGE_LOOP ( 'NONE', ( #15732, #23056, #17766, #7708 ) ) ;
#17652 = DIRECTION ( 'NONE',  ( 1.000000000000000000, 7.703719777548943412E-32, 0.000000000000000000 ) ) ;
#17653 = VERTEX_POINT ( 'NONE', #2590 ) ;
#17654 = CARTESIAN_POINT ( 'NONE',  ( 60.15393183416158962, 5.971812294485358663, 16.58880310854675599 ) ) ;
#17655 = CARTESIAN_POINT ( 'NONE',  ( -70.55000000109247082, 8.538419263543522320, 16.46158073645647235 ) ) ;
#17656 = CARTESIAN_POINT ( 'NONE',  ( 72.50000000000000000, 9.999999999999998224, 14.99999999999999645 ) ) ;
#17657 = ORIENTED_EDGE ( 'NONE', *, *, #4796, .F. ) ;
#17658 = DIRECTION ( 'NONE',  ( 1.000000000000000000, -0.000000000000000000, -1.224646799147353207E-16 ) ) ;
#17659 = ORIENTED_EDGE ( 'NONE', *, *, #22166, .T. ) ;
#17660 = CARTESIAN_POINT ( 'NONE',  ( -2.828427124746189403, 2.828427124746190291, 19.87500000000001066 ) ) ;
#17661 = ORIENTED_EDGE ( 'NONE', *, *, #4095, .T. ) ;
#17662 = CARTESIAN_POINT ( 'NONE',  ( 55.15856816583844591, 7.028187705514647554, 16.31069182806492179 ) ) ;
#17663 = CARTESIAN_POINT ( 'NONE',  ( -65.85000000218495586, 11.03553390593273598, 12.49999999999999289 ) ) ;
#17664 = FACE_OUTER_BOUND ( 'NONE', #8312, .T. ) ;
#17665 = DIRECTION ( 'NONE',  ( 1.000000000000000000, 7.703719777548943412E-32, 0.000000000000000000 ) ) ;
#17666 = CARTESIAN_POINT ( 'NONE',  ( 1.432654583217643163, -3.458734124999999882, 15.00000000136560807 ) ) ;
#17667 = CARTESIAN_POINT ( 'NONE',  ( -1.656854249492380138, -3.999999999999999112, 15.31250000273119660 ) ) ;
#17668 = DIRECTION ( 'NONE',  ( -1.000000000000000000, 0.000000000000000000, 0.000000000000000000 ) ) ;
#17669 = CARTESIAN_POINT ( 'NONE',  ( 67.09999999999999432, 7.499999999999996447, 14.99999999999999645 ) ) ;
#17670 = CARTESIAN_POINT ( 'NONE',  ( 57.37500000000000000, 7.878679656440349177, 12.87867965644035984 ) ) ;
#17671 = CARTESIAN_POINT ( 'NONE',  ( -3.458734125000000770, 1.432654583217640498, 2.925000001365598123 ) ) ;
#17672 = CARTESIAN_POINT ( 'NONE',  ( -1.432654583217639832, -3.458734125000000326, 11.87500000136560452 ) ) ;
#17673 = CARTESIAN_POINT ( 'NONE',  ( -69.50000000109245946, 10.85617417291294551, 12.93301269999999192 ) ) ;
#17674 = VERTEX_POINT ( 'NONE', #2363 ) ;
#17675 = DIRECTION ( 'NONE',  ( 1.000000000000000000, 0.000000000000000000, 0.000000000000000000 ) ) ;
#17676 = CARTESIAN_POINT ( 'NONE',  ( -4.175002511812151873, -2.208363329454905877, -3.469254087858246738 ) ) ;
#17677 = EDGE_LOOP ( 'NONE', ( #23669, #17053, #6708, #15700 ) ) ;
#17678 = DIRECTION ( 'NONE',  ( -1.000000000000000000, -0.000000000000000000, -0.000000000000000000 ) ) ;
#17679 = CARTESIAN_POINT ( 'NONE',  ( -2.828427124746189403, -2.828427124746190735, 1.550000002731187765 ) ) ;
#17680 = ORIENTED_EDGE ( 'NONE', *, *, #7397, .T. ) ;
#17681 = ORIENTED_EDGE ( 'NONE', *, *, #19737, .F. ) ;
#17682 = ADVANCED_FACE ( 'NONE', ( #14985 ), #22604, .F. ) ;
#17683 = DIRECTION ( 'NONE',  ( 0.000000000000000000, 0.3090169943749482284, -0.9510565162951534202 ) ) ;
#17684 = DIRECTION ( 'NONE',  ( 0.000000000000000000, 0.000000000000000000, -1.000000000000000000 ) ) ;
#17685 = VERTEX_POINT ( 'NONE', #9810 ) ;
#17686 = DIRECTION ( 'NONE',  ( 0.000000000000000000, 0.000000000000000000, 1.000000000000000000 ) ) ;
#17687 = UNCERTAINTY_MEASURE_WITH_UNIT (LENGTH_MEASURE( 1.000000000000000082E-05 ), #19455, 'distance_accuracy_value', 'NONE');
#17688 = CARTESIAN_POINT ( 'NONE',  ( -69.55000000218493028, 7.499999999999996447, 16.03553390593273775 ) ) ;
#17689 = EDGE_CURVE ( 'NONE', #8676, #1478, #9409, .T. ) ;
#17690 = LINE ( 'NONE', #21246, #1803 ) ;
#17691 = CARTESIAN_POINT ( 'NONE',  ( 72.35000000000000853, 12.50000000000000000, 16.03553390593273420 ) ) ;
#17692 = CIRCLE ( 'NONE', #6217, 0.2500000000000002220 ) ;
#17693 = FACE_OUTER_BOUND ( 'NONE', #20270, .T. ) ;
#17694 = CARTESIAN_POINT ( 'NONE',  ( 4.999999999999999112, -4.472189673936844301, 8.264486777890091673 ) ) ;
#17695 =( BOUNDED_CURVE ( )  B_SPLINE_CURVE ( 2, ( #3474, #6608, #4794, #1417, #23471, #19871, #18085, #3117, #19750 ),
 .UNSPECIFIED., .F., .F. ) 
 B_SPLINE_CURVE_WITH_KNOTS ( ( 3, 2, 2, 2, 3 ),
 ( 0.8749999999999990008, 0.8906249999999994449, 0.9062499999999998890, 0.9218750000000003331, 0.9375000000000007772 ),
 .UNSPECIFIED. ) 
 CURVE ( )  GEOMETRIC_REPRESENTATION_ITEM ( )  RATIONAL_B_SPLINE_CURVE ( ( 1.000000000000004885, 0.9238795325112818535, 1.000000000000000000, 0.9238795325112867385, 1.000000000000000000, 0.9238795325112867385, 1.000000000000000000, 0.9238795325112829637, 1.000000000000003775 ) ) 
 REPRESENTATION_ITEM ( '' )  );
#17696 = CARTESIAN_POINT ( 'NONE',  ( 55.53356816583845301, 11.72490539043803004, 18.97181229448534268 ) ) ;
#17697 = CARTESIAN_POINT ( 'NONE',  ( 6.353591512924457348E-16, -3.458734125000000326, 3.987500001365595015 ) ) ;
#17698 = CARTESIAN_POINT ( 'NONE',  ( -2.445694354108819191, 2.445694354108820523, 15.31250000136560452 ) ) ;
#17699 = DIRECTION ( 'NONE',  ( 1.000000000000000000, -0.000000000000000000, -0.000000000000000000 ) ) ;
#17700 = LINE ( 'NONE', #7157, #18193 ) ;
#17701 = ORIENTED_EDGE ( 'NONE', *, *, #19807, .F. ) ;
#17702 = CARTESIAN_POINT ( 'NONE',  ( -2.977338099904818236, 2.250880586719687493, 2.039999999999999591 ) ) ;
#17703 = CARTESIAN_POINT ( 'NONE',  ( -6.500000000000000000, 3.752776749732573247, -3.119443416399232394 ) ) ;
#17704 = CARTESIAN_POINT ( 'NONE',  ( -4.000000000000000000, 0.000000000000000000, -1.699999999999998401 ) ) ;
#17705 = EDGE_LOOP ( 'NONE', ( #23647, #5723 ) ) ;
#17706 = EDGE_CURVE ( 'NONE', #17992, #4647, #5558, .T. ) ;
#17707 = DIRECTION ( 'NONE',  ( 0.000000000000000000, 0.000000000000000000, 1.000000000000000000 ) ) ;
#17708 = DIRECTION ( 'NONE',  ( 0.3420201433256622181, 0.9396926207859107594, -6.162975822039141593E-32 ) ) ;
#17709 = ADVANCED_FACE ( 'NONE', ( #17233 ), #6327, .T. ) ;
#17710 = DIRECTION ( 'NONE',  ( 0.000000000000000000, 0.000000000000000000, 1.000000000000000000 ) ) ;
#17711 = ORIENTED_EDGE ( 'NONE', *, *, #21922, .F. ) ;
#17712 = CARTESIAN_POINT ( 'NONE',  ( -68.50000000218494733, 11.76776695296636888, 16.76776695296636532 ) ) ;
#17713 = ORIENTED_EDGE ( 'NONE', *, *, #18855, .F. ) ;
#17714 = CARTESIAN_POINT ( 'NONE',  ( 54.46875000000000000, 5.999999999999987566, 13.34314575050763452 ) ) ;
#17715 = EDGE_CURVE ( 'NONE', #7167, #7410, #1378, .T. ) ;
#17716 = CARTESIAN_POINT ( 'NONE',  ( 68.65000000218496723, 8.964466094067258695, 17.50000000000000355 ) ) ;
#17717 = EDGE_CURVE ( 'NONE', #15133, #2790, #11313, .T. ) ;
#17718 = CARTESIAN_POINT ( 'NONE',  ( 3.007318562400188799, 2.637429632093199139, 2.039999999999998259 ) ) ;
#17719 = DIRECTION ( 'NONE',  ( -0.000000000000000000, 0.000000000000000000, -1.000000000000000000 ) ) ;
#17720 = CARTESIAN_POINT ( 'NONE',  ( 68.25000000109245946, 9.999999999999998224, 17.06698730000000097 ) ) ;
#17721 = ORIENTED_EDGE ( 'NONE', *, *, #2903, .T. ) ;
#17722 = CARTESIAN_POINT ( 'NONE',  ( 4.000000000000000888, 4.898587196589412829E-16, -20.00000000000000000 ) ) ;
#17723 = FACE_OUTER_BOUND ( 'NONE', #14934, .T. ) ;
#17724 = CARTESIAN_POINT ( 'NONE',  ( 67.30000000109247082, 12.06698730000000275, 15.85617417291294196 ) ) ;
#17725 = CARTESIAN_POINT ( 'NONE',  ( -1.432654583217638944, 3.458734125000000326, 11.25000000136560452 ) ) ;
#17726 = DIRECTION ( 'NONE',  ( -1.000000000000000000, -0.000000000000000000, -0.000000000000000000 ) ) ;
#17727 = DIRECTION ( 'NONE',  ( -0.5000000000000007772, -0.8660254037844382635, 0.000000000000000000 ) ) ;
#17728 = VERTEX_POINT ( 'NONE', #19590 ) ;
#17729 = CARTESIAN_POINT ( 'NONE',  ( 44.09522139676619901, -9.000000000000007105, 5.000000000000079936 ) ) ;
#17730 = VECTOR ( 'NONE', #149, 1000.000000000000000 ) ;
#17731 = CARTESIAN_POINT ( 'NONE',  ( 59.34375000000000711, 8.757359312880723223, 18.00000000000000711 ) ) ;
#17732 = CARTESIAN_POINT ( 'NONE',  ( 66.84999999999999432, 11.03553390593268624, 17.50000000000005329 ) ) ;
#17733 = ORIENTED_EDGE ( 'NONE', *, *, #5366, .F. ) ;
#17734 = CARTESIAN_POINT ( 'NONE',  ( 5.432802636760778903, -4.368923434677197903, -0.2573354458087873109 ) ) ;
#17735 = CARTESIAN_POINT ( 'NONE',  ( 0.000000000000000000, 0.000000000000000000, 0.000000000000000000 ) ) ;
#17736 = ADVANCED_FACE ( 'NONE', ( #3076 ), #11854, .T. ) ;
#17737 = ORIENTED_EDGE ( 'NONE', *, *, #12027, .T. ) ;
#17738 = DIRECTION ( 'NONE',  ( 0.000000000000000000, -0.3090169943749349057, -0.9510565162951575280 ) ) ;
#17739 = ORIENTED_EDGE ( 'NONE', *, *, #15839, .F. ) ;
#17740 = CARTESIAN_POINT ( 'NONE',  ( -19.99999999999999645, -15.00000000000001954, 10.00000000000008882 ) ) ;
#17741 = CLOSED_SHELL ( 'NONE', ( #608, #22380, #12591, #4241, #7770 ) ) ;
#17742 = ORIENTED_EDGE ( 'NONE', *, *, #20672, .F. ) ;
#17743 = CARTESIAN_POINT ( 'NONE',  ( 1.025207404391860050E-15, 3.458734125000000770, 11.43750000136560452 ) ) ;
#17744 = DIRECTION ( 'NONE',  ( 0.000000000000000000, 0.000000000000000000, 1.000000000000000000 ) ) ;
#17745 = EDGE_CURVE ( 'NONE', #9843, #1357, #17586, .T. ) ;
#17746 = DIRECTION ( 'NONE',  ( -7.087422195345011518E-32, -1.000000000000000000, 0.000000000000000000 ) ) ;
#17747 = DIRECTION ( 'NONE',  ( -1.000000000000000000, 0.000000000000000000, 0.000000000000000000 ) ) ;
#17748 = DIRECTION ( 'NONE',  ( 0.000000000000000000, 0.000000000000000000, -1.000000000000000000 ) ) ;
#17749 = CARTESIAN_POINT ( 'NONE',  ( -69.49999999999998579, 7.499999999999996447, 14.99999999999999645 ) ) ;
#17750 = CARTESIAN_POINT ( 'NONE',  ( 50.00000000000000000, -10.00000000000001954, 12.50000000000002665 ) ) ;
#17751 = CARTESIAN_POINT ( 'NONE',  ( 59.99999999999182876, 10.99015334700498236, 18.43425161108635280 ) ) ;
#17752 = CARTESIAN_POINT ( 'NONE',  ( -1.432654583217641164, -3.458734125000000326, 0.1750000013655959585 ) ) ;
#17753 = CARTESIAN_POINT ( 'NONE',  ( -67.40000000218495302, 9.999999999999998224, 12.49999999999999289 ) ) ;
#17754 = CARTESIAN_POINT ( 'NONE',  ( -66.09999999999999432, 9.999999999999998224, 17.49999999999999645 ) ) ;
#17755 = CARTESIAN_POINT ( 'NONE',  ( 1.872352939448454495E-15, -3.458734125000000326, 15.68750000136560629 ) ) ;
#17756 = LINE ( 'NONE', #6741, #2300 ) ;
#17757 = ORIENTED_EDGE ( 'NONE', *, *, #17715, .T. ) ;
#17758 = CARTESIAN_POINT ( 'NONE',  ( -3.999999999999998224, -1.656854249492383024, 14.18750000273119660 ) ) ;
#17759 = ORIENTED_EDGE ( 'NONE', *, *, #14815, .T. ) ;
#17760 = CARTESIAN_POINT ( 'NONE',  ( 59.12268183416157541, 12.78030770151606177, 17.87654654797631792 ) ) ;
#17761 = CARTESIAN_POINT ( 'NONE',  ( -67.80000000109247082, 12.06698730000000275, 14.14382582708705094 ) ) ;
#17762 = DIRECTION ( 'NONE',  ( 1.000000000000000000, 0.000000000000000000, 0.000000000000000000 ) ) ;
#17763 = CARTESIAN_POINT ( 'NONE',  ( -2.445694354108819635, -2.445694354108820523, -3.137499998634404541 ) ) ;
#17764 = ORIENTED_EDGE ( 'NONE', *, *, #19288, .F. ) ;
#17765 = LINE ( 'NONE', #4597, #1823 ) ;
#17766 = ORIENTED_EDGE ( 'NONE', *, *, #13112, .F. ) ;
#17767 = DIRECTION ( 'NONE',  ( -1.000000000000000000, -0.000000000000000000, -0.000000000000000000 ) ) ;
#17768 = EDGE_LOOP ( 'NONE', ( #8575, #1782, #3317, #7040 ) ) ;
#17769 = EDGE_CURVE ( 'NONE', #14518, #14298, #6340, .T. ) ;
#17770 = CARTESIAN_POINT ( 'NONE',  ( 54.68981816583844591, 9.931948859054354983, 11.99999999999999645 ) ) ;
#17771 = AXIS2_PLACEMENT_3D ( 'NONE', #3523, #16231, #6770 ) ;
#17772 = CARTESIAN_POINT ( 'NONE',  ( -68.45000000218493597, 12.50000000000000000, 16.03553390593273420 ) ) ;
#17773 = CARTESIAN_POINT ( 'NONE',  ( -1.489200000000000301, 0.000000000000000000, 0.000000000000000000 ) ) ;
#17774 = CARTESIAN_POINT ( 'NONE',  ( -72.20000000109246230, 10.85617417291294551, 17.06698729999999742 ) ) ;
#17775 = CARTESIAN_POINT ( 'NONE',  ( 1.872352939448454495E-15, -3.458734125000000770, 14.93750000136560452 ) ) ;
#17776 = CARTESIAN_POINT ( 'NONE',  ( -1.656854249492380138, -3.999999999999999112, 10.31250000273119483 ) ) ;
#17777 = FACE_OUTER_BOUND ( 'NONE', #9825, .T. ) ;
#17778 = LINE ( 'NONE', #1230, #14845 ) ;
#17779 = CARTESIAN_POINT ( 'NONE',  ( 56.81250000000000000, 13.00000000000000000, 14.99999999999998757 ) ) ;
#17780 = CARTESIAN_POINT ( 'NONE',  ( 3.458734125000000770, 4.235727675282972223E-16, 2.487500001365596791 ) ) ;
#17781 = CARTESIAN_POINT ( 'NONE',  ( 0.6867006470895935522, -3.397451134755354207, 2.039999999999998703 ) ) ;
#17782 = DIRECTION ( 'NONE',  ( 0.000000000000000000, 0.000000000000000000, 1.000000000000000000 ) ) ;
#17783 = VECTOR ( 'NONE', #21419, 1000.000000000000000 ) ;
#17784 = ORIENTED_EDGE ( 'NONE', *, *, #7212, .T. ) ;
#17785 = DIRECTION ( 'NONE',  ( -1.000000000000000000, 0.000000000000000000, 0.000000000000000000 ) ) ;
#17786 = CARTESIAN_POINT ( 'NONE',  ( 4.999999999999999112, -6.807171995660539210, -6.478011392632959442 ) ) ;
#17787 = ORIENTED_EDGE ( 'NONE', *, *, #8357, .F. ) ;
#17788 = CARTESIAN_POINT ( 'NONE',  ( 58.78125000000000711, 8.757359312880703683, 11.99999999999999822 ) ) ;
#17789 = AXIS2_PLACEMENT_3D ( 'NONE', #15510, #20627, #4235 ) ;
#17790 =( NAMED_UNIT ( * ) PLANE_ANGLE_UNIT ( ) SI_UNIT ( $, .RADIAN. ) );
#17791 = CARTESIAN_POINT ( 'NONE',  ( 4.000000000000000000, 1.656854249492381248, -0.01249999726881388662 ) ) ;
#17792 = FACE_OUTER_BOUND ( 'NONE', #4029, .T. ) ;
#17793 = ORIENTED_EDGE ( 'NONE', *, *, #21984, .F. ) ;
#17794 = VERTEX_POINT ( 'NONE', #19240 ) ;
#17795 = CARTESIAN_POINT ( 'NONE',  ( 2.974182810908596597, -5.788408252967910173, 3.144609816681590009E-17 ) ) ;
#17796 = CARTESIAN_POINT ( 'NONE',  ( 70.89999999999999147, 9.999999999999998224, 17.49999999999999645 ) ) ;
#17797 = ORIENTED_EDGE ( 'NONE', *, *, #14235, .T. ) ;
#17798 = DIRECTION ( 'NONE',  ( -0.000000000000000000, -0.000000000000000000, -1.000000000000000000 ) ) ;
#17799 = CARTESIAN_POINT ( 'NONE',  ( 4.000000000000000888, 1.656854249492381248, 11.56250000000001066 ) ) ;
#17800 = CARTESIAN_POINT ( 'NONE',  ( 66.10000000109248219, 10.85617417291294551, 12.93301269999999370 ) ) ;
#17801 = CARTESIAN_POINT ( 'NONE',  ( 71.79999999999998295, 8.232233047033627571, 16.76776695296636532 ) ) ;
#17802 = PRODUCT_RELATED_PRODUCT_CATEGORY ( 'part', '', ( #15290 ) ) ;
#17803 = VECTOR ( 'NONE', #7156, 1000.000000000000000 ) ;
#17804 = LINE ( 'NONE', #4866, #1670 ) ;
#17805 = EDGE_CURVE ( 'NONE', #18995, #22965, #6793, .T. ) ;
#17806 = CARTESIAN_POINT ( 'NONE',  ( 4.000000000000000000, 0.000000000000000000, 0.000000000000000000 ) ) ;
#17807 = CARTESIAN_POINT ( 'NONE',  ( 52.78125000000000711, 8.343145750507600766, 11.00000000000000533 ) ) ;
#17808 = CARTESIAN_POINT ( 'NONE',  ( 1.432654583217639832, 3.458734125000000326, 3.425000001365596791 ) ) ;
#17809 = CARTESIAN_POINT ( 'NONE',  ( 3.458734125000002102, -1.432654583217639610, 12.87500000136560629 ) ) ;
#17810 = CARTESIAN_POINT ( 'NONE',  ( 68.15000000218495302, 8.964466094067214286, 12.50000000000004086 ) ) ;
#17811 = DIRECTION ( 'NONE',  ( -0.000000000000000000, -1.000000000000000000, -0.000000000000000000 ) ) ;
#17812 = ORIENTED_EDGE ( 'NONE', *, *, #12706, .T. ) ;
#17813 = CARTESIAN_POINT ( 'NONE',  ( -6.989194030332740226, -11.25000000000000355, 10.00000000000008882 ) ) ;
#17814 = DIRECTION ( 'NONE',  ( 4.625929269271486900E-16, -1.000000000000000000, -5.665129472695380173E-32 ) ) ;
#17815 = DIRECTION ( 'NONE',  ( 1.000000000000000000, 0.000000000000000000, 0.000000000000000000 ) ) ;
#17816 = ADVANCED_FACE ( 'NONE', ( #6445, #15685 ), #1260, .T. ) ;
#17817 = ORIENTED_EDGE ( 'NONE', *, *, #1168, .T. ) ;
#17818 = DIRECTION ( 'NONE',  ( 1.000000000000000000, -0.000000000000000000, -0.000000000000000000 ) ) ;
#17819 = CARTESIAN_POINT ( 'NONE',  ( -67.35000000000000853, 11.03553390593276973, 12.50000000000002665 ) ) ;
#17820 = AXIS2_PLACEMENT_3D ( 'NONE', #17656, #6748, #10722 ) ;
#17821 = CARTESIAN_POINT ( 'NONE',  ( 59.43750000000000711, 10.00000000000001776, 18.99999999999999645 ) ) ;
#17822 = ORIENTED_EDGE ( 'NONE', *, *, #7446, .T. ) ;
#17823 = CYLINDRICAL_SURFACE ( 'NONE', #16795, 8.749000000000002331 ) ;
#17824 = VERTEX_POINT ( 'NONE', #6566 ) ;
#17825 = CARTESIAN_POINT ( 'NONE',  ( 55.12500000000000711, 12.82842712474620228, 17.82842712474617386 ) ) ;
#17826 = CARTESIAN_POINT ( 'NONE',  ( 67.60000000218495586, 12.50000000000000000, 14.99999999999999645 ) ) ;
#17827 = DIRECTION ( 'NONE',  ( 0.000000000000000000, 0.000000000000000000, 1.000000000000000000 ) ) ;
#17828 = FACE_OUTER_BOUND ( 'NONE', #565, .T. ) ;
#17829 = CARTESIAN_POINT ( 'NONE',  ( -4.000000000000000000, -1.656854249492383024, -0.6374999999999969580 ) ) ;
#17830 = EDGE_LOOP ( 'NONE', ( #16055, #23563, #22671, #1131, #21290, #11995, #15075, #7324, #8953, #13742, #7487, #5179, #3229, #10922, #17701, #5096, #4440, #8601, #11803, #10368, #23472, #307, #2092, #22814, #22035, #14390, #23248, #13515, #7905, #5794, #5090, #21940, #6595, #19464, #6985, #22369, #14601, #23026, #13196, #7910, #5468, #6351, #21708, #21243, #5060, #11392, #14394, #72, #15469, #4741, #15399, #4675, #10096, #20085, #6718, #18006, #10974, #3439, #22953, #21863, #5236, #22464, #2284, #18659, #17029, #14644, #10579, #3142, #12700, #14396, #8692, #12178, #10776, #5119, #3879, #15838, #11300, #23375, #13490, #1106, #1195, #5472, #11514, #9628, #10892 ) ) ;
#17831 = EDGE_CURVE ( 'NONE', #16726, #3210, #10378, .T. ) ;
#17832 = DIRECTION ( 'NONE',  ( 0.000000000000000000, 0.8660254037844380415, -0.5000000000000012212 ) ) ;
#17833 = ADVANCED_FACE ( 'NONE', ( #16023 ), #20904, .F. ) ;
#17834 = DIRECTION ( 'NONE',  ( 1.000000000000000000, -0.000000000000000000, -1.224646799147353207E-16 ) ) ;
#17835 = CARTESIAN_POINT ( 'NONE',  ( 67.25000000109245946, 12.06698730000000097, 14.99999999999999645 ) ) ;
#17836 = CARTESIAN_POINT ( 'NONE',  ( 1.432654583217643163, -3.458734124999999882, 18.00000000136560274 ) ) ;
#17837 = CARTESIAN_POINT ( 'NONE',  ( 2.500000000000000000, -1.178949249685214307, 2.042000000000001592 ) ) ;
#17838 = LINE ( 'NONE', #6706, #2716 ) ;
#17839 = ORIENTED_EDGE ( 'NONE', *, *, #5962, .F. ) ;
#17840 = CYLINDRICAL_SURFACE ( 'NONE', #17354, 11.00000000000000000 ) ;
#17841 = CARTESIAN_POINT ( 'NONE',  ( 55.59375000000002132, 11.24264068711927322, 11.99999999999998934 ) ) ;
#17842 = CARTESIAN_POINT ( 'NONE',  ( 66.90000000000000568, 9.999999999999998224, 17.49999999999999645 ) ) ;
#17843 = DIRECTION ( 'NONE',  ( 1.000000000000000000, 0.000000000000000000, 0.000000000000000000 ) ) ;
#17844 = EDGE_CURVE ( 'NONE', #299, #2926, #18559, .T. ) ;
#17845 = VERTEX_POINT ( 'NONE', #3186 ) ;
#17846 = CYLINDRICAL_SURFACE ( 'NONE', #2082, 2.500000000000002220 ) ;
#17847 = CARTESIAN_POINT ( 'NONE',  ( 2.445694354108820523, -2.445694354108820079, -0.8874999986344025427 ) ) ;
#17848 = CARTESIAN_POINT ( 'NONE',  ( 2.687328764639642653, -3.067272167851299969, -0.05923475698271395140 ) ) ;
#17849 = EDGE_LOOP ( 'NONE', ( #4913, #11360, #16209, #8175, #21744, #8557 ) ) ;
#17850 = LINE ( 'NONE', #10813, #2894 ) ;
#17851 = EDGE_LOOP ( 'NONE', ( #13680, #19872, #10505, #2185 ) ) ;
#17852 = CARTESIAN_POINT ( 'NONE',  ( 4.000000000000000888, 1.656854249492381248, 12.68750000273119660 ) ) ;
#17853 = VERTEX_POINT ( 'NONE', #11974 ) ;
#17854 = CARTESIAN_POINT ( 'NONE',  ( -3.999999999999999112, 0.000000000000000000, 18.00000000000001066 ) ) ;
#17855 = DIRECTION ( 'NONE',  ( 1.000000000000000000, 0.000000000000000000, 0.000000000000000000 ) ) ;
#17856 = CARTESIAN_POINT ( 'NONE',  ( -65.95000000109247651, 8.538419263543524096, 13.53841926354352054 ) ) ;
#17857 = ADVANCED_FACE ( 'NONE', ( #4871 ), #10177, .T. ) ;
#17858 = CARTESIAN_POINT ( 'NONE',  ( 65.95000000109247651, 8.538419263543524096, 13.53841926354352054 ) ) ;
#17859 = DIRECTION ( 'NONE',  ( 0.000000000000000000, 0.000000000000000000, 1.000000000000000000 ) ) ;
#17860 = CARTESIAN_POINT ( 'NONE',  ( -71.50000000000000000, 12.50000000000000000, 14.99999999999999645 ) ) ;
#17861 = EDGE_CURVE ( 'NONE', #21099, #18371, #19354, .T. ) ;
#17862 = CARTESIAN_POINT ( 'NONE',  ( 5.200000000000002842, 0.000000000000000000, 0.000000000000000000 ) ) ;
#17863 = CARTESIAN_POINT ( 'NONE',  ( 60.00000000000000711, 13.77581299381601099, 16.13248257417277642 ) ) ;
#17864 = AXIS2_PLACEMENT_3D ( 'NONE', #20383, #20139, #10967 ) ;
#17865 = CARTESIAN_POINT ( 'NONE',  ( 1.432654583217642275, -3.458734124999999882, -1.699999998634404097 ) ) ;
#17866 = CARTESIAN_POINT ( 'NONE',  ( 0.000000000000000000, -9.680994141368808314, 5.222868219166821646 ) ) ;
#17867 = CARTESIAN_POINT ( 'NONE',  ( 68.30000000218494449, 11.76776695296636888, 13.23223304703362579 ) ) ;
#17868 = CARTESIAN_POINT ( 'NONE',  ( -3.458734124999998993, -1.432654583217642497, 17.50000000136560274 ) ) ;
#17869 = DIRECTION ( 'NONE',  ( -0.000000000000000000, 1.000000000000000000, -0.000000000000000000 ) ) ;
#17870 = ADVANCED_FACE ( 'NONE', ( #23068 ), #6679, .F. ) ;
#17871 = ADVANCED_FACE ( 'NONE', ( #9079 ), #1854, .T. ) ;
#17872 = ORIENTED_EDGE ( 'NONE', *, *, #2671, .T. ) ;
#17873 = VECTOR ( 'NONE', #10615, 1000.000000000000114 ) ;
#17874 = CARTESIAN_POINT ( 'NONE',  ( -16.41397198033274307, -11.25000000000000355, 10.00000000000008882 ) ) ;
#17875 = EDGE_LOOP ( 'NONE', ( #21161, #3259, #3421, #1416 ) ) ;
#17876 = CARTESIAN_POINT ( 'NONE',  ( 58.93518183416157541, 9.931948859054379852, 18.99999999999999289 ) ) ;
#17877 = CARTESIAN_POINT ( 'NONE',  ( -67.30000000109247082, 9.143825827087049163, 17.06698729999999742 ) ) ;
#17878 = CARTESIAN_POINT ( 'NONE',  ( 1.432654583217639832, 3.458734125000000326, -1.574999998634403875 ) ) ;
#17879 = VERTEX_POINT ( 'NONE', #14595 ) ;
#17880 = FACE_OUTER_BOUND ( 'NONE', #17651, .T. ) ;
#17881 = EDGE_LOOP ( 'NONE', ( #1868, #7971, #6493, #14365 ) ) ;
#17882 = CYLINDRICAL_SURFACE ( 'NONE', #22821, 2.500000000000002220 ) ;
#17883 = ORIENTED_EDGE ( 'NONE', *, *, #1436, .F. ) ;
#17884 = CARTESIAN_POINT ( 'NONE',  ( 51.31481816583844591, 12.99999999999999822, 14.93194885905435676 ) ) ;
#17885 = CARTESIAN_POINT ( 'NONE',  ( -68.35000000218495586, 12.50000000000000000, 13.96446609406725869 ) ) ;
#17886 = CARTESIAN_POINT ( 'NONE',  ( -3.999999999999999112, 0.000000000000000000, 14.12500000273119660 ) ) ;
#17887 = AXIS2_PLACEMENT_3D ( 'NONE', #15814, #825, #15705 ) ;
#17888 = DIRECTION ( 'NONE',  ( 1.000000000000000000, 0.000000000000000000, 0.000000000000000000 ) ) ;
#17889 = CARTESIAN_POINT ( 'NONE',  ( -1.432654583217639166, 3.458734125000000770, 17.50000000136560274 ) ) ;
#17890 = LINE ( 'NONE', #14317, #20644 ) ;
#17891 = CARTESIAN_POINT ( 'NONE',  ( 56.53125000000000711, 11.24264068711929276, 18.00000000000000355 ) ) ;
#17892 = LINE ( 'NONE', #21578, #13683 ) ;
#17893 = VECTOR ( 'NONE', #20451, 1000.000000000000114 ) ;
#17894 = ADVANCED_FACE ( 'NONE', ( #10651 ), #18392, .T. ) ;
#17895 = CARTESIAN_POINT ( 'NONE',  ( 51.78356816583844591, 8.689308171935074654, 12.02818770551464489 ) ) ;
#17896 = CARTESIAN_POINT ( 'NONE',  ( -1.432654583217640498, 3.458734125000000770, -0.1999999986344043745 ) ) ;
#17897 = DIRECTION ( 'NONE',  ( 0.000000000000000000, 0.000000000000000000, -1.000000000000000000 ) ) ;
#17898 = EDGE_CURVE ( 'NONE', #10786, #7079, #6992, .T. ) ;
#17899 = DIRECTION ( 'NONE',  ( 1.000000000000000000, 0.000000000000000000, 0.000000000000000000 ) ) ;
#17900 = EDGE_CURVE ( 'NONE', #4288, #21750, #16603, .T. ) ;
#17901 = ORIENTED_EDGE ( 'NONE', *, *, #21498, .F. ) ;
#17902 = CARTESIAN_POINT ( 'NONE',  ( 1.025207404391860050E-15, 3.458734125000000326, 10.18750000136560629 ) ) ;
#17903 = CARTESIAN_POINT ( 'NONE',  ( -3.540020015735593439, -2.810662092924100630, -3.602146406945814672 ) ) ;
#17904 = VERTEX_POINT ( 'NONE', #23665 ) ;
#17905 = CARTESIAN_POINT ( 'NONE',  ( -35.00000000000000711, 4.500000000000001776, -49.99999999999998579 ) ) ;
#17906 = CARTESIAN_POINT ( 'NONE',  ( -2.449293598294706907E-16, 4.000000000000000000, 1.175000002731187543 ) ) ;
#17907 = CARTESIAN_POINT ( 'NONE',  ( -8.706242640716551406, -8.974600000000002353, 5.000000000000079936 ) ) ;
#17908 = ORIENTED_EDGE ( 'NONE', *, *, #2501, .F. ) ;
#17909 = ORIENTED_EDGE ( 'NONE', *, *, #16249, .T. ) ;
#17910 = DIRECTION ( 'NONE',  ( 0.8660254037844385966, 0.000000000000000000, 0.5000000000000001110 ) ) ;
#17911 = DIRECTION ( 'NONE',  ( -1.000000000000000000, -0.000000000000000000, -0.000000000000000000 ) ) ;
#17912 = VERTEX_POINT ( 'NONE', #3308 ) ;
#17913 = CYLINDRICAL_SURFACE ( 'NONE', #1491, 4.000000000000000000 ) ;
#17914 = AXIS2_PLACEMENT_3D ( 'NONE', #1339, #4601, #4950 ) ;
#17915 = AXIS2_PLACEMENT_3D ( 'NONE', #23256, #6866, #988 ) ;
#17916 = CARTESIAN_POINT ( 'NONE',  ( -2.828427124746188515, -2.828427124746190735, 12.12500000000001066 ) ) ;
#17917 = LINE ( 'NONE', #8707, #9104 ) ;
#17918 = CARTESIAN_POINT ( 'NONE',  ( 66.00000000109245946, 7.933012699999995476, 15.85617417291294196 ) ) ;
#17919 = CARTESIAN_POINT ( 'NONE',  ( -65.50000000218494733, 8.232233047033627571, 16.76776695296636532 ) ) ;
#17920 = AXIS2_PLACEMENT_3D ( 'NONE', #13077, #20334, #11273 ) ;
#17921 = FACE_OUTER_BOUND ( 'NONE', #19172, .T. ) ;
#17922 = CARTESIAN_POINT ( 'NONE',  ( 58.62731816583843170, 12.87654654797634102, 17.78030770151602979 ) ) ;
#17923 = CARTESIAN_POINT ( 'NONE',  ( 3.458734125000000770, -1.432654583217639610, 5.175000001365595459 ) ) ;
#17924 = CYLINDRICAL_SURFACE ( 'NONE', #4566, 5.000000000000011546 ) ;
#17925 = CARTESIAN_POINT ( 'NONE',  ( 3.458734125000001214, 4.235727675282971730E-16, 14.93750000136560452 ) ) ;
#17926 = CARTESIAN_POINT ( 'NONE',  ( 1.656854249492380138, 4.000000000000000000, -0.01249999999999832148 ) ) ;
#17927 = CARTESIAN_POINT ( 'NONE',  ( -68.49999999999998579, 9.999999999999998224, 17.49999999999999645 ) ) ;
#17928 = ORIENTED_EDGE ( 'NONE', *, *, #17613, .T. ) ;
#17929 = CARTESIAN_POINT ( 'NONE',  ( 2.000000000000000000, 0.000000000000000000, -6.200000000000021494 ) ) ;
#17930 = VECTOR ( 'NONE', #437, 1000.000000000000000 ) ;
#17931 = CARTESIAN_POINT ( 'NONE',  ( 0.000000000000000000, -5.538577986808947529, 6.772677083992368452 ) ) ;
#17932 = DIRECTION ( 'NONE',  ( -1.000000000000000000, 0.000000000000000000, 0.000000000000000000 ) ) ;
#17933 = ORIENTED_EDGE ( 'NONE', *, *, #17831, .T. ) ;
#17934 = CARTESIAN_POINT ( 'NONE',  ( 45.00000000000000000, 14.69846310392956745, 35.82846581308617573 ) ) ;
#17935 = ORIENTED_EDGE ( 'NONE', *, *, #8210, .F. ) ;
#17936 = AXIS2_PLACEMENT_3D ( 'NONE', #7693, #22263, #7804 ) ;
#17937 = CARTESIAN_POINT ( 'NONE',  ( 71.15000000218496723, 7.499999999999996447, 16.03553390593273775 ) ) ;
#17938 = EDGE_LOOP ( 'NONE', ( #2062, #23259, #5736, #4737 ) ) ;
#17939 = ORIENTED_EDGE ( 'NONE', *, *, #1266, .T. ) ;
#17940 = AXIS2_PLACEMENT_3D ( 'NONE', #17948, #1528, #1879 ) ;
#17941 = EDGE_CURVE ( 'NONE', #5492, #21989, #12798, .T. ) ;
#17942 = CARTESIAN_POINT ( 'NONE',  ( 51.75000000000000711, 7.171572875253819923, 17.82842712474619873 ) ) ;
#17943 = CARTESIAN_POINT ( 'NONE',  ( 67.30000000218494449, 8.232233047033629347, 13.23223304703362402 ) ) ;
#17944 = AXIS2_PLACEMENT_3D ( 'NONE', #6861, #1690, #14185 ) ;
#17945 = DIRECTION ( 'NONE',  ( 1.000000000000000000, 0.000000000000000000, 0.000000000000000000 ) ) ;
#17946 = VECTOR ( 'NONE', #18268, 1000.000000000000114 ) ;
#17947 = CARTESIAN_POINT ( 'NONE',  ( 50.00000000000000000, 15.00000000000003375, 34.11836509645780069 ) ) ;
#17948 = CARTESIAN_POINT ( 'NONE',  ( -4.898587196589412829E-16, 0.000000000000000000, -4.000000000000000000 ) ) ;
#17949 = ORIENTED_EDGE ( 'NONE', *, *, #20871, .F. ) ;
#17950 = CARTESIAN_POINT ( 'NONE',  ( -6.989194030332740226, -11.25000000000000355, 10.00000000000008882 ) ) ;
#17951 = CARTESIAN_POINT ( 'NONE',  ( 57.43518183416157541, 9.931948859054379852, 18.99999999999999289 ) ) ;
#17952 = CARTESIAN_POINT ( 'NONE',  ( -2.828427124746189403, -2.828427124746190735, -1.449999997268811347 ) ) ;
#17953 = CARTESIAN_POINT ( 'NONE',  ( 67.10000000109246798, 10.85617417291294551, 12.93301269999999370 ) ) ;
#17954 = CARTESIAN_POINT ( 'NONE',  ( 1.025207404391860050E-15, 3.458734125000000326, 10.18750000136560629 ) ) ;
#17955 = DIRECTION ( 'NONE',  ( 0.3420201433256622181, 0.9396926207859107594, -6.162975822039141593E-32 ) ) ;
#17956 = AXIS2_PLACEMENT_3D ( 'NONE', #8872, #3568, #10904 ) ;
#17957 = DIRECTION ( 'NONE',  ( 0.000000000000000000, 0.000000000000000000, 1.000000000000000000 ) ) ;
#17958 = ORIENTED_EDGE ( 'NONE', *, *, #10708, .F. ) ;
#17959 = CARTESIAN_POINT ( 'NONE',  ( 68.49999999999998579, 9.999999999999998224, 17.49999999999999645 ) ) ;
#17960 = CARTESIAN_POINT ( 'NONE',  ( 57.09375000000000711, 11.24264068711927322, 11.99999999999998934 ) ) ;
#17961 = CARTESIAN_POINT ( 'NONE',  ( 4.000000000000000888, 1.656854249492381248, 10.68750000273119483 ) ) ;
#17962 = ORIENTED_EDGE ( 'NONE', *, *, #8261, .F. ) ;
#17963 = DIRECTION ( 'NONE',  ( 7.087422195345011518E-32, 1.000000000000000000, -0.000000000000000000 ) ) ;
#17964 = CARTESIAN_POINT ( 'NONE',  ( 2.445694354108820523, -2.445694354108820079, -1.887499998634403431 ) ) ;
#17965 = DIRECTION ( 'NONE',  ( 0.000000000000000000, 0.000000000000000000, -1.000000000000000000 ) ) ;
#17966 = VECTOR ( 'NONE', #18130, 1000.000000000000000 ) ;
#17967 = ORIENTED_EDGE ( 'NONE', *, *, #7862, .F. ) ;
#17968 = CARTESIAN_POINT ( 'NONE',  ( 1.489200000000000079, 0.000000000000000000, 0.000000000000000000 ) ) ;
#17969 = EDGE_LOOP ( 'NONE', ( #1043, #18, #19085, #6802 ) ) ;
#17970 = EDGE_CURVE ( 'NONE', #4949, #12476, #673, .T. ) ;
#17971 = DIRECTION ( 'NONE',  ( -1.000000000000000000, 0.000000000000000000, -0.000000000000000000 ) ) ;
#17972 =( BOUNDED_CURVE ( )  B_SPLINE_CURVE ( 3, ( #9540, #7145, #10980, #7270 ),
 .UNSPECIFIED., .F., .F. ) 
 B_SPLINE_CURVE_WITH_KNOTS ( ( 4, 4 ),
 ( 5.501996899079006020, 6.283185307179586232 ),
 .UNSPECIFIED. ) 
 CURVE ( )  GEOMETRIC_REPRESENTATION_ITEM ( )  RATIONAL_B_SPLINE_CURVE ( ( 1.000000000000000000, 0.9497886580611611951, 0.9497886580611611951, 1.000000000000000000 ) ) 
 REPRESENTATION_ITEM ( '' )  );
#17973 = EDGE_CURVE ( 'NONE', #5711, #14744, #21497, .T. ) ;
#17974 = CARTESIAN_POINT ( 'NONE',  ( 2.828427124746192067, -2.828427124746189847, 18.37500000000001066 ) ) ;
#17975 = DIRECTION ( 'NONE',  ( 0.000000000000000000, -6.982962677686266711E-15, 1.000000000000000000 ) ) ;
#17976 = AXIS2_PLACEMENT_3D ( 'NONE', #20549, #7653, #16868 ) ;
#17977 = AXIS2_PLACEMENT_3D ( 'NONE', #3303, #18152, #16366 ) ;
#17978 = CARTESIAN_POINT ( 'NONE',  ( 0.000000000000000000, -1.178949249685214307, 2.042000000000001592 ) ) ;
#17979 = EDGE_CURVE ( 'NONE', #23527, #17305, #6711, .T. ) ;
#17980 = CARTESIAN_POINT ( 'NONE',  ( 34.99999999999999289, 7.500000000000001776, -50.00000000000000000 ) ) ;
#17981 = AXIS2_PLACEMENT_3D ( 'NONE', #8602, #14357, #21501 ) ;
#17982 = CARTESIAN_POINT ( 'NONE',  ( -67.34999999999999432, 11.03553390593273598, 12.49999999999999289 ) ) ;
#17983 = VECTOR ( 'NONE', #5770, 1000.000000000000000 ) ;
#17984 = CARTESIAN_POINT ( 'NONE',  ( 66.55000000218494449, 8.964466094067294222, 12.49999999999996092 ) ) ;
#17985 = DIRECTION ( 'NONE',  ( -0.000000000000000000, -1.000000000000000000, -0.000000000000000000 ) ) ;
#17986 = CARTESIAN_POINT ( 'NONE',  ( 70.90000000218495302, 11.76776695296636888, 16.76776695296636532 ) ) ;
#17987 = CARTESIAN_POINT ( 'NONE',  ( -1.432654583217640498, 3.458734125000000770, -0.1999999986344043745 ) ) ;
#17988 = CARTESIAN_POINT ( 'NONE',  ( 0.7185353092834488864, -8.974600000000002353, 5.000000000000079936 ) ) ;
#17989 = CARTESIAN_POINT ( 'NONE',  ( 68.05000000000001137, 8.964466094067256918, 12.49999999999999822 ) ) ;
#17990 = CARTESIAN_POINT ( 'NONE',  ( -1.432654583217639610, -3.458734124999999882, 16.62500000136560629 ) ) ;
#17991 = CARTESIAN_POINT ( 'NONE',  ( -66.30000000218494449, 8.232233047033627571, 16.76776695296636532 ) ) ;
#17992 = VERTEX_POINT ( 'NONE', #20168 ) ;
#17993 = CARTESIAN_POINT ( 'NONE',  ( -71.70000000109247651, 10.85617417291294551, 12.93301269999999192 ) ) ;
#17994 = ORIENTED_EDGE ( 'NONE', *, *, #12316, .T. ) ;
#17995 = CARTESIAN_POINT ( 'NONE',  ( 54.43518183416157541, 9.931948859054379852, 18.99999999999999289 ) ) ;
#17996 = CARTESIAN_POINT ( 'NONE',  ( -67.25000000109247367, 9.999999999999998224, 17.06698730000000097 ) ) ;
#17997 =( LENGTH_UNIT ( ) NAMED_UNIT ( * ) SI_UNIT ( .MILLI., .METRE. ) );
#17998 = CARTESIAN_POINT ( 'NONE',  ( 3.458734125000001214, -1.432654583217639610, -2.824999998634404541 ) ) ;
#17999 = VERTEX_POINT ( 'NONE', #19704 ) ;
#18000 = AXIS2_PLACEMENT_3D ( 'NONE', #3829, #7797, #16648 ) ;
#18001 = CYLINDRICAL_SURFACE ( 'NONE', #19400, 4.000000000000002665 ) ;
#18002 = EDGE_CURVE ( 'NONE', #22874, #3756, #3433, .T. ) ;
#18003 = EDGE_CURVE ( 'NONE', #12149, #23165, #16259, .T. ) ;
#18004 = ORIENTED_EDGE ( 'NONE', *, *, #396, .T. ) ;
#18005 = DIRECTION ( 'NONE',  ( -1.000000000000000000, -0.000000000000000000, -0.000000000000000000 ) ) ;
#18006 = ORIENTED_EDGE ( 'NONE', *, *, #16451, .F. ) ;
#18007 = CARTESIAN_POINT ( 'NONE',  ( 59.71875000000000711, 13.00000000000000711, 16.24264068711927322 ) ) ;
#18008 = CARTESIAN_POINT ( 'NONE',  ( -65.60000000218495586, 7.499999999999996447, 14.99999999999999645 ) ) ;
#18009 = EDGE_CURVE ( 'NONE', #10792, #11370, #21736, .T. ) ;
#18010 = LINE ( 'NONE', #23145, #12163 ) ;
#18011 = EDGE_CURVE ( 'NONE', #23216, #19381, #12480, .T. ) ;
#18012 =( BOUNDED_CURVE ( )  B_SPLINE_CURVE ( 2, ( #645, #6050, #17315, #9902, #15061, #20649, #17196, #2442, #8107 ),
 .UNSPECIFIED., .F., .F. ) 
 B_SPLINE_CURVE_WITH_KNOTS ( ( 3, 2, 2, 2, 3 ),
 ( 0.8499999999999999778, 0.8625000000000000444, 0.8750000000000000000, 0.8874999999999999556, 0.9000000000000000222 ),
 .UNSPECIFIED. ) 
 CURVE ( )  GEOMETRIC_REPRESENTATION_ITEM ( )  RATIONAL_B_SPLINE_CURVE ( ( 1.000000000000000000, 0.9238795325112867385, 1.000000000000000000, 0.9238795325112867385, 1.000000000000000000, 0.9238795325112867385, 1.000000000000000000, 0.9238795325112867385, 1.000000000000000000 ) ) 
 REPRESENTATION_ITEM ( '' )  );
#18013 = CARTESIAN_POINT ( 'NONE',  ( 3.458734125000001658, 1.432654583217640498, 17.25000000136560629 ) ) ;
#18014 = CYLINDRICAL_SURFACE ( 'NONE', #12217, 2.500000000000002220 ) ;
#18015 = CARTESIAN_POINT ( 'NONE',  ( -20.00000000000000355, 4.500000000000003553, 2.449293598294706907E-15 ) ) ;
#18016 = CARTESIAN_POINT ( 'NONE',  ( 67.24999999999998579, 8.964466094067294222, 12.49999999999996092 ) ) ;
#18017 = CARTESIAN_POINT ( 'NONE',  ( 50.84606816583843880, 8.825410453826357582, 18.02818770551464667 ) ) ;
#18018 = CARTESIAN_POINT ( 'NONE',  ( -2.445694354108819635, -2.445694354108820967, -1.887499998634403431 ) ) ;
#18019 = CARTESIAN_POINT ( 'NONE',  ( -3.999999999999998224, -1.656854249492383246, 18.18750000273119483 ) ) ;
#18020 = CARTESIAN_POINT ( 'NONE',  ( 70.60000000218494165, 9.999999999999998224, 12.49999999999999289 ) ) ;
#18021 = ORIENTED_EDGE ( 'NONE', *, *, #22231, .F. ) ;
#18022 = CARTESIAN_POINT ( 'NONE',  ( 70.50000000000000000, 9.999999999999998224, 12.49999999999999289 ) ) ;
#18023 = PLANE ( 'NONE',  #17771 ) ;
#18024 = EDGE_LOOP ( 'NONE', ( #1453, #3551 ) ) ;
#18025 = CARTESIAN_POINT ( 'NONE',  ( 53.71875000000002132, 13.00000000000000711, 16.24264068711927322 ) ) ;
#18026 = FILL_AREA_STYLE ('',( #16468 ) ) ;
#18027 = CARTESIAN_POINT ( 'NONE',  ( 2.828427124746190735, -2.828427124746189847, 1.800000002731187987 ) ) ;
#18028 = CARTESIAN_POINT ( 'NONE',  ( 45.00000000000000000, -2.399706452296378245, 55.00000000000021316 ) ) ;
#18029 = VERTEX_POINT ( 'NONE', #18159 ) ;
#18030 = CARTESIAN_POINT ( 'NONE',  ( 1.656854249492384135, -3.999999999999999112, 17.31250000000001421 ) ) ;
#18031 = ORIENTED_EDGE ( 'NONE', *, *, #6885, .T. ) ;
#18032 = ADVANCED_FACE ( 'NONE', ( #1741 ), #5462, .F. ) ;
#18033 = CARTESIAN_POINT ( 'NONE',  ( 69.25000000000000000, 11.03553390593269157, 17.50000000000004619 ) ) ;
#18034 = ORIENTED_EDGE ( 'NONE', *, *, #8764, .T. ) ;
#18035 = CARTESIAN_POINT ( 'NONE',  ( 32.14370665323380649, -9.000000000000001776, 10.00000000000008882 ) ) ;
#18036 = CARTESIAN_POINT ( 'NONE',  ( -3.999999999999999112, 1.656854249492380804, 11.93750000000001066 ) ) ;
#18037 = EDGE_CURVE ( 'NONE', #20184, #18556, #15538, .T. ) ;
#18038 = ORIENTED_EDGE ( 'NONE', *, *, #9696, .F. ) ;
#18039 = DIRECTION ( 'NONE',  ( 0.3420201433256622736, -0.9396926207859106484, -1.232595164407828100E-31 ) ) ;
#18040 = EDGE_CURVE ( 'NONE', #4247, #19246, #22079, .T. ) ;
#18041 = CARTESIAN_POINT ( 'NONE',  ( 70.59999999999999432, 11.76776695296636888, 13.23223304703362579 ) ) ;
#18042 = CARTESIAN_POINT ( 'NONE',  ( 6.500000000000000000, 3.752776749732563477, -3.700000000000000178 ) ) ;
#18043 = CARTESIAN_POINT ( 'NONE',  ( 69.65000000218496723, 7.499999999999996447, 13.96446609406725514 ) ) ;
#18044 = CARTESIAN_POINT ( 'NONE',  ( 56.75231816583843170, 7.219692298483957771, 17.87654654797633924 ) ) ;
#18045 = CARTESIAN_POINT ( 'NONE',  ( -3.458734124999999882, -1.432654583217642497, 1.800000001365597235 ) ) ;
#18046 = DIRECTION ( 'NONE',  ( 0.000000000000000000, 0.000000000000000000, 1.000000000000000000 ) ) ;
#18047 = CARTESIAN_POINT ( 'NONE',  ( -1.432654583217639610, -3.458734124999999882, 13.62500000136560452 ) ) ;
#18048 = DIRECTION ( 'NONE',  ( -1.000000000000000000, 0.000000000000000000, 0.000000000000000000 ) ) ;
#18049 = CARTESIAN_POINT ( 'NONE',  ( 55.00000000000000711, -15.00000000000000000, 10.00000000000000000 ) ) ;
#18050 = VERTEX_POINT ( 'NONE', #4016 ) ;
#18051 = DIRECTION ( 'NONE',  ( -0.3420201433256622181, 0.9396926207859106484, 1.232595164407828100E-31 ) ) ;
#18052 = DIRECTION ( 'NONE',  ( -1.000000000000000000, -0.000000000000000000, -0.000000000000000000 ) ) ;
#18053 = CARTESIAN_POINT ( 'NONE',  ( 118.3095189484530181, 2.399706452296379577, 55.00000000000021316 ) ) ;
#18054 = VERTEX_POINT ( 'NONE', #4373 ) ;
#18055 = VERTEX_POINT ( 'NONE', #2211 ) ;
#18056 = CARTESIAN_POINT ( 'NONE',  ( 4.999999999999999112, -6.478011392632939014, 6.807171995660559638 ) ) ;
#18057 = DIRECTION ( 'NONE',  ( 0.000000000000000000, 0.000000000000000000, 1.000000000000000000 ) ) ;
#18058 = ORIENTED_EDGE ( 'NONE', *, *, #11500, .F. ) ;
#18059 = LINE ( 'NONE', #20304, #1088 ) ;
#18060 = ORIENTED_EDGE ( 'NONE', *, *, #10135, .T. ) ;
#18061 = CARTESIAN_POINT ( 'NONE',  ( 55.21875000000000000, 14.00000000000000888, 16.65685424949235482 ) ) ;
#18062 = EDGE_CURVE ( 'NONE', #19580, #2340, #7632, .T. ) ;
#18063 = CARTESIAN_POINT ( 'NONE',  ( 66.75000000218494733, 12.50000000000000000, 13.96446609406725869 ) ) ;
#18064 = CARTESIAN_POINT ( 'NONE',  ( 2.000000000000001776, 0.000000000000000000, 6.543750000000017053 ) ) ;
#18065 = CARTESIAN_POINT ( 'NONE',  ( 66.49999999999998579, 9.999999999999998224, 12.49999999999999289 ) ) ;
#18066 = CARTESIAN_POINT ( 'NONE',  ( -3.999999999999999112, 0.000000000000000000, 12.12500000273119838 ) ) ;
#18067 = ORIENTED_EDGE ( 'NONE', *, *, #14702, .T. ) ;
#18068 = CARTESIAN_POINT ( 'NONE',  ( -3.999999999999999112, 1.656854249492380804, 16.06250000273119838 ) ) ;
#18069 = LINE ( 'NONE', #1649, #9177 ) ;
#18070 = CARTESIAN_POINT ( 'NONE',  ( 60.81018183416157541, 14.00000000000000000, 15.06805114094561304 ) ) ;
#18071 = CARTESIAN_POINT ( 'NONE',  ( 35.00000000000000000, 7.500000000000001776, -20.00000000000000355 ) ) ;
#18072 = CARTESIAN_POINT ( 'NONE',  ( 4.999999999999999112, 0.000000000000000000, 0.000000000000000000 ) ) ;
#18073 = CARTESIAN_POINT ( 'NONE',  ( -69.20000000000000284, 11.76776695296636888, 16.76776695296636532 ) ) ;
#18074 = CARTESIAN_POINT ( 'NONE',  ( 4.999999999999999112, 8.152713396088763886, 3.174628368996105010 ) ) ;
#18075 = ORIENTED_EDGE ( 'NONE', *, *, #3448, .F. ) ;
#18076 = DIRECTION ( 'NONE',  ( 1.000000000000000000, -0.000000000000000000, -0.000000000000000000 ) ) ;
#18077 = CARTESIAN_POINT ( 'NONE',  ( 57.93750000000000000, 10.00000000000000711, 17.99999999999999645 ) ) ;
#18078 = CARTESIAN_POINT ( 'NONE',  ( -3.028668353233797905, -9.000000000000003553, 5.000000000000079936 ) ) ;
#18079 = CIRCLE ( 'NONE', #14969, 11.00000000000000000 ) ;
#18080 = EDGE_LOOP ( 'NONE', ( #15881, #10015, #8494, #21210 ) ) ;
#18081 = CARTESIAN_POINT ( 'NONE',  ( -1.799999999999996048, 0.000000000000000000, -6.000000000000021316 ) ) ;
#18082 = CARTESIAN_POINT ( 'NONE',  ( -2.445694354108820523, 2.445694354108820523, -3.387499998634403209 ) ) ;
#18083 = FACE_OUTER_BOUND ( 'NONE', #20487, .T. ) ;
#18084 = ORIENTED_EDGE ( 'NONE', *, *, #1004, .F. ) ;
#18085 = CARTESIAN_POINT ( 'NONE',  ( -65.90000000218495302, 11.76776695296636888, 13.23223304703362579 ) ) ;
#18086 = ORIENTED_EDGE ( 'NONE', *, *, #22120, .F. ) ;
#18087 = LINE ( 'NONE', #1784, #4892 ) ;
#18088 = CARTESIAN_POINT ( 'NONE',  ( 4.000000000000000888, 1.656854249492381248, 18.56250000000001421 ) ) ;
#18089 = CARTESIAN_POINT ( 'NONE',  ( -66.40000000000000568, 8.232233047033629347, 13.23223304703362402 ) ) ;
#18090 = DIRECTION ( 'NONE',  ( 0.000000000000000000, 0.000000000000000000, 1.000000000000000000 ) ) ;
#18091 = CARTESIAN_POINT ( 'NONE',  ( 40.13469571966727045, -11.25000000000000355, 10.00000000000008882 ) ) ;
#18092 = CARTESIAN_POINT ( 'NONE',  ( 72.15000000109247935, 9.999999999999998224, 17.49999999999999645 ) ) ;
#18093 = VECTOR ( 'NONE', #13380, 1000.000000000000114 ) ;
#18094 = CARTESIAN_POINT ( 'NONE',  ( -66.64999999999999147, 12.50000000000000000, 13.96446609406725869 ) ) ;
#18095 = VECTOR ( 'NONE', #23277, 1000.000000000000000 ) ;
#18096 = DIRECTION ( 'NONE',  ( -1.000000000000000000, 0.000000000000000000, 0.000000000000000000 ) ) ;
#18097 = CARTESIAN_POINT ( 'NONE',  ( 2.000000000000000000, 7.592810154713616459E-16, 6.200000000000021494 ) ) ;
#18098 = DIRECTION ( 'NONE',  ( 1.000000000000000000, 0.000000000000000000, 0.000000000000000000 ) ) ;
#18099 = EDGE_CURVE ( 'NONE', #18050, #4939, #18943, .T. ) ;
#18100 = CARTESIAN_POINT ( 'NONE',  ( 2.828427124746190735, -2.828427124746189847, 3.675000000000002931 ) ) ;
#18101 = CARTESIAN_POINT ( 'NONE',  ( 7.347880794884118750E-16, -4.000000000000000000, 0.5500000000000018208 ) ) ;
#18102 = DIRECTION ( 'NONE',  ( -1.000000000000000000, 0.000000000000000000, 0.000000000000000000 ) ) ;
#18103 = CARTESIAN_POINT ( 'NONE',  ( -1.432654583217638944, 3.458734125000000326, 16.25000000136560629 ) ) ;
#18104 = CARTESIAN_POINT ( 'NONE',  ( 25.24566549676620397, -9.000000000000001776, 10.00000000000008882 ) ) ;
#18105 = EDGE_LOOP ( 'NONE', ( #9818, #17496, #11005, #12045 ) ) ;
#18106 = CARTESIAN_POINT ( 'NONE',  ( -68.85000000109248219, 9.999999999999998224, 17.06698730000000097 ) ) ;
#18107 = VERTEX_POINT ( 'NONE', #18977 ) ;
#18108 = CARTESIAN_POINT ( 'NONE',  ( 53.02893183416157541, 11.58880310854676132, 19.02818770551463956 ) ) ;
#18109 = CARTESIAN_POINT ( 'NONE',  ( -67.35000000109248219, 8.538419263543522320, 16.46158073645647235 ) ) ;
#18110 = CARTESIAN_POINT ( 'NONE',  ( 27.50000000000000000, -3.499999999999989342, -33.66025403784446723 ) ) ;
#18111 =( BOUNDED_CURVE ( )  B_SPLINE_CURVE ( 2, ( #14522, #1551, #7082, #14399, #21662, #21786, #5393, #3477, #12733 ),
 .UNSPECIFIED., .F., .F. ) 
 B_SPLINE_CURVE_WITH_KNOTS ( ( 3, 2, 2, 2, 3 ),
 ( 0.1000000000000000056, 0.1125000000000000028, 0.1250000000000000000, 0.1375000000000000111, 0.1499999999999999944 ),
 .UNSPECIFIED. ) 
 CURVE ( )  GEOMETRIC_REPRESENTATION_ITEM ( )  RATIONAL_B_SPLINE_CURVE ( ( 1.000000000000000000, 0.9238795325112867385, 1.000000000000000000, 0.9238795325112867385, 1.000000000000000000, 0.9238795325112867385, 1.000000000000000000, 0.9238795325112867385, 1.000000000000000000 ) ) 
 REPRESENTATION_ITEM ( '' )  );
#18112 = EDGE_CURVE ( 'NONE', #3848, #21099, #17203, .T. ) ;
#18113 = FACE_OUTER_BOUND ( 'NONE', #20667, .T. ) ;
#18114 = EDGE_LOOP ( 'NONE', ( #522, #2400, #15371, #14309 ) ) ;
#18115 = VECTOR ( 'NONE', #18978, 1000.000000000000000 ) ;
#18116 = CIRCLE ( 'NONE', #19251, 4.000000000000001776 ) ;
#18117 = VERTEX_POINT ( 'NONE', #18754 ) ;
#18118 = DIRECTION ( 'NONE',  ( -0.000000000000000000, -1.000000000000000000, -0.000000000000000000 ) ) ;
#18119 = CARTESIAN_POINT ( 'NONE',  ( 58.96875000000000711, 6.999999999999992895, 13.75735931288071967 ) ) ;
#18120 = CARTESIAN_POINT ( 'NONE',  ( -69.80000000109247082, 7.933012699999995476, 15.85617417291294196 ) ) ;
#18121 = CARTESIAN_POINT ( 'NONE',  ( -68.45000000109247651, 7.933012699999995476, 14.99999999999999645 ) ) ;
#18122 = CARTESIAN_POINT ( 'NONE',  ( 1.432654583217641386, 3.458734125000000770, 14.37500000136560452 ) ) ;
#18123 = CARTESIAN_POINT ( 'NONE',  ( -2.828427124746189403, 2.828427124746190291, 11.00000000273119660 ) ) ;
#18124 = CARTESIAN_POINT ( 'NONE',  ( 54.75000000000000711, 7.878679656440361612, 17.12132034355964549 ) ) ;
#18125 = DIRECTION ( 'NONE',  ( 0.000000000000000000, 0.000000000000000000, 1.000000000000000000 ) ) ;
#18126 = EDGE_CURVE ( 'NONE', #7757, #8256, #22584, .T. ) ;
#18127 = CARTESIAN_POINT ( 'NONE',  ( 55.96875000000000000, 6.999999999999992895, 13.75735931288071967 ) ) ;
#18128 = EDGE_CURVE ( 'NONE', #8065, #10786, #15266, .T. ) ;
#18129 = CARTESIAN_POINT ( 'NONE',  ( 2.828427124746191179, 2.828427124746190291, 18.75000000273119483 ) ) ;
#18130 = DIRECTION ( 'NONE',  ( 0.000000000000000000, 0.000000000000000000, -1.000000000000000000 ) ) ;
#18131 = ORIENTED_EDGE ( 'NONE', *, *, #20866, .T. ) ;
#18132 = CARTESIAN_POINT ( 'NONE',  ( -3.999999999999999112, 0.000000000000000000, 16.00000000000001066 ) ) ;
#18133 = LINE ( 'NONE', #19803, #6305 ) ;
#18134 = ORIENTED_EDGE ( 'NONE', *, *, #18167, .F. ) ;
#18135 = CARTESIAN_POINT ( 'NONE',  ( 55.03125000000000000, 11.24264068711929276, 18.00000000000000355 ) ) ;
#18136 = CARTESIAN_POINT ( 'NONE',  ( -1.656854249492381248, -3.999999999999999112, -3.387499997268812901 ) ) ;
#18137 = EDGE_CURVE ( 'NONE', #12645, #9405, #16751, .T. ) ;
#18138 = CARTESIAN_POINT ( 'NONE',  ( 72.50000000000000000, 9.999999999999998224, 12.49999999999999289 ) ) ;
#18139 = ORIENTED_EDGE ( 'NONE', *, *, #21361, .T. ) ;
#18140 = CARTESIAN_POINT ( 'NONE',  ( -1.656854249492380138, -3.999999999999999112, 16.18750000000001066 ) ) ;
#18141 = VERTEX_POINT ( 'NONE', #20560 ) ;
#18142 = CARTESIAN_POINT ( 'NONE',  ( -3.729367062499998831, 0.000000000000000000, 19.28125000204840234 ) ) ;
#18143 = CARTESIAN_POINT ( 'NONE',  ( -2.828427124746190291, 2.828427124746190291, -2.699999997268812457 ) ) ;
#18144 = ORIENTED_EDGE ( 'NONE', *, *, #10920, .F. ) ;
#18145 = CARTESIAN_POINT ( 'NONE',  ( 0.000000000000000000, 4.729683950898872169, 7.360373001730934561 ) ) ;
#18146 = CARTESIAN_POINT ( 'NONE',  ( 4.999999999999999112, 7.593217523260583413, 7.958834565716794707 ) ) ;
#18147 = CARTESIAN_POINT ( 'NONE',  ( 4.000000000000000000, 0.1981133338132474442, 2.382280164152719704E-17 ) ) ;
#18148 = CARTESIAN_POINT ( 'NONE',  ( 70.79999999999999716, 11.76776695296636888, 16.76776695296636532 ) ) ;
#18149 = EDGE_CURVE ( 'NONE', #13840, #8586, #564, .T. ) ;
#18150 = CARTESIAN_POINT ( 'NONE',  ( 4.999999999999999112, 0.000000000000000000, 0.000000000000000000 ) ) ;
#18152 = DIRECTION ( 'NONE',  ( -1.000000000000000000, 0.000000000000000000, 1.224646799147353207E-16 ) ) ;
#18151 = VECTOR ( 'NONE', #5552, 1000.000000000000000 ) ;
#18153 = CARTESIAN_POINT ( 'NONE',  ( 55.62731816583843170, 12.87654654797634102, 17.78030770151602979 ) ) ;
#18154 = ADVANCED_FACE ( 'NONE', ( #5968 ), #16318, .T. ) ;
#18155 = AXIS2_PLACEMENT_3D ( 'NONE', #15123, #713, #2625 ) ;
#18156 = CARTESIAN_POINT ( 'NONE',  ( -3.458734125000000326, 0.000000000000000000, 1.737500001365596347 ) ) ;
#18157 =( NAMED_UNIT ( * ) SI_UNIT ( $, .STERADIAN. ) SOLID_ANGLE_UNIT ( ) );
#18158 = CARTESIAN_POINT ( 'NONE',  ( 1.432654583217643163, -3.458734124999999437, 10.75000000136560452 ) ) ;
#18159 = CARTESIAN_POINT ( 'NONE',  ( 6.500000000000000888, 0.000000000000000000, -3.700000000000000178 ) ) ;
#18160 = DIRECTION ( 'NONE',  ( 0.3420201433256622736, -0.9396926207859106484, -1.232595164407828100E-31 ) ) ;
#18161 = ORIENTED_EDGE ( 'NONE', *, *, #943, .F. ) ;
#18162 = CARTESIAN_POINT ( 'NONE',  ( -3.999999999999999112, 1.656854249492380582, 12.06250000273119838 ) ) ;
#18163 = DIRECTION ( 'NONE',  ( 1.000000000000000000, 7.703719777548943412E-32, 0.000000000000000000 ) ) ;
#18164 = PLANE ( 'NONE',  #6690 ) ;
#18165 = EDGE_CURVE ( 'NONE', #23216, #14554, #1338, .T. ) ;
#18166 = ORIENTED_EDGE ( 'NONE', *, *, #2344, .T. ) ;
#18167 = EDGE_CURVE ( 'NONE', #5335, #13481, #20844, .T. ) ;
#18168 = EDGE_LOOP ( 'NONE', ( #12705, #14126, #16379 ) ) ;
#18169 = CYLINDRICAL_SURFACE ( 'NONE', #14841, 8.749000000000002331 ) ;
#18170 = CARTESIAN_POINT ( 'NONE',  ( 56.06250000000000000, 5.999999999999996447, 15.00000000000001599 ) ) ;
#18171 = ORIENTED_EDGE ( 'NONE', *, *, #6502, .F. ) ;
#18172 = CARTESIAN_POINT ( 'NONE',  ( 2.828427124746192067, -2.828427124746189847, 18.37500000000001066 ) ) ;
#18173 = EDGE_LOOP ( 'NONE', ( #21683, #17872, #9152, #209 ) ) ;
#18174 = CARTESIAN_POINT ( 'NONE',  ( 54.37500000000000711, 7.171572875253794166, 12.17157287525381726 ) ) ;
#18175 = SHAPE_REPRESENTATION ( 'Gripper Jaw with Integrated Rack', ( #7318 ), #28 ) ;
#18176 = VECTOR ( 'NONE', #15796, 1000.000000000000000 ) ;
#18177 = CARTESIAN_POINT ( 'NONE',  ( 68.80000000218494449, 7.499999999999996447, 14.99999999999999645 ) ) ;
#18178 = CARTESIAN_POINT ( 'NONE',  ( 15.83013239071656741, -8.974600000000002353, 5.000000000000079936 ) ) ;
#18179 = CARTESIAN_POINT ( 'NONE',  ( 66.90000000000000568, 9.999999999999998224, 17.49999999999999645 ) ) ;
#18180 = CARTESIAN_POINT ( 'NONE',  ( 50.38765154071656838, -8.974600000000002353, 5.000000000000079936 ) ) ;
#18181 = ORIENTED_EDGE ( 'NONE', *, *, #12604, .F. ) ;
#18182 = CARTESIAN_POINT ( 'NONE',  ( -3.999999999999998224, -1.656854249492383246, 17.18750000273119838 ) ) ;
#18183 =( REPRESENTATION_RELATIONSHIP ('NONE','NONE', #8403, #6707 ) REPRESENTATION_RELATIONSHIP_WITH_TRANSFORMATION ( #9983 )SHAPE_REPRESENTATION_RELATIONSHIP( ) );
#18184 = PLANE ( 'NONE',  #739 ) ;
#18185 = CARTESIAN_POINT ( 'NONE',  ( 58.56018183416157541, 5.999999999999996447, 14.93194885905437808 ) ) ;
#18186 = CARTESIAN_POINT ( 'NONE',  ( -16.41397198033274307, -11.25000000000000355, 10.00000000000008882 ) ) ;
#18187 = CARTESIAN_POINT ( 'NONE',  ( 49.55947366966726264, -11.25000000000000355, 5.000000000000079936 ) ) ;
#18188 = CARTESIAN_POINT ( 'NONE',  ( -68.95000000000000284, 11.03553390593269157, 12.49999999999994849 ) ) ;
#18189 = CIRCLE ( 'NONE', #7876, 0.03079999999999923077 ) ;
#18190 = EDGE_LOOP ( 'NONE', ( #13871, #15590, #16096, #14228 ) ) ;
#18191 = CARTESIAN_POINT ( 'NONE',  ( 1.236993788156008760E-15, 0.000000000000000000, 21.31370849898476649 ) ) ;
#18192 = CARTESIAN_POINT ( 'NONE',  ( 55.68750000000000000, 9.999999999999989342, 11.99999999999999467 ) ) ;
#18193 = VECTOR ( 'NONE', #12693, 1000.000000000000000 ) ;
#18194 = DIRECTION ( 'NONE',  ( -1.000000000000000000, -0.000000000000000000, -0.000000000000000000 ) ) ;
#18195 = EDGE_CURVE ( 'NONE', #16998, #21720, #9586, .T. ) ;
#18196 = ADVANCED_FACE ( 'NONE', ( #19241 ), #19130, .F. ) ;
#18197 = ORIENTED_EDGE ( 'NONE', *, *, #20638, .F. ) ;
#18198 = CARTESIAN_POINT ( 'NONE',  ( 3.250000000000001776, -5.629165124598848990, 1.734723475976807094E-15 ) ) ;
#18199 = CARTESIAN_POINT ( 'NONE',  ( -5.384454397937118664, 6.702023979852544604E-16, -5.000000000000000000 ) ) ;
#18200 = CARTESIAN_POINT ( 'NONE',  ( 0.000000000000000000, 0.000000000000000000, 0.000000000000000000 ) ) ;
#18201 = ORIENTED_EDGE ( 'NONE', *, *, #12899, .T. ) ;
#18202 = CYLINDRICAL_SURFACE ( 'NONE', #11064, 2.649999999999992806 ) ;
#18203 = EDGE_LOOP ( 'NONE', ( #5498, #8915 ) ) ;
#18204 = VECTOR ( 'NONE', #18163, 1000.000000000000000 ) ;
#18205 = ORIENTED_EDGE ( 'NONE', *, *, #5716, .T. ) ;
#18206 = CARTESIAN_POINT ( 'NONE',  ( 0.000000000000000000, 3.399999999999999911, 2.039999999999998259 ) ) ;
#18207 = CARTESIAN_POINT ( 'NONE',  ( 1.656854249492381470, 4.000000000000000000, 18.68750000000001066 ) ) ;
#18208 = CARTESIAN_POINT ( 'NONE',  ( 19.99999999999999289, 9.999999999999964473, -20.00000000000000355 ) ) ;
#18209 = CARTESIAN_POINT ( 'NONE',  ( -65.00000000000000000, 15.00000000000000000, 20.00000000000001421 ) ) ;
#18210 = DIRECTION ( 'NONE',  ( -1.000000000000000000, -7.703719777548943412E-32, 0.000000000000000000 ) ) ;
#18211 = DIRECTION ( 'NONE',  ( 1.000000000000000000, 0.000000000000000000, 0.000000000000000000 ) ) ;
#18212 = CARTESIAN_POINT ( 'NONE',  ( -67.14999999999999147, 7.499999999999995559, 13.96446609406725692 ) ) ;
#18213 = CARTESIAN_POINT ( 'NONE',  ( -90.00000000000000000, 0.000000000000000000, -8.265000000000021885 ) ) ;
#18214 = CARTESIAN_POINT ( 'NONE',  ( -3.458734124999998993, 0.000000000000000000, 16.43750000136560629 ) ) ;
#18215 = CARTESIAN_POINT ( 'NONE',  ( -1.240299975428113101E-15, -4.647091401871173311, -3.572172305156514849 ) ) ;
#18216 = CARTESIAN_POINT ( 'NONE',  ( 2.445694354108820967, -2.445694354108820079, -2.637499998634404097 ) ) ;
#18217 = CARTESIAN_POINT ( 'NONE',  ( -1.665216334060555692, 3.652639802690383242, 9.999838423880746063 ) ) ;
#18218 = CARTESIAN_POINT ( 'NONE',  ( 1.025207404391860050E-15, 3.458734125000000326, 12.18750000136560629 ) ) ;
#18219 = CARTESIAN_POINT ( 'NONE',  ( -12.45344630323380208, -9.000000000000003553, 5.000000000000079936 ) ) ;
#18220 = ORIENTED_EDGE ( 'NONE', *, *, #17613, .F. ) ;
#18221 = CARTESIAN_POINT ( 'NONE',  ( -70.45000000109247651, 9.999999999999998224, 17.06698730000000097 ) ) ;
#18222 = ORIENTED_EDGE ( 'NONE', *, *, #1037, .T. ) ;
#18223 = CARTESIAN_POINT ( 'NONE',  ( 55.84143183416158251, 8.275094609562001935, 18.97181229448536044 ) ) ;
#18224 = CARTESIAN_POINT ( 'NONE',  ( -66.85000000109248219, 9.999999999999998224, 12.93301269999999192 ) ) ;
#18225 = DIRECTION ( 'NONE',  ( 0.000000000000000000, 0.000000000000000000, 1.000000000000000000 ) ) ;
#18226 = CARTESIAN_POINT ( 'NONE',  ( 4.000000000000000888, 4.898587196589412829E-16, 17.50000000000001066 ) ) ;
#18227 = VERTEX_POINT ( 'NONE', #22959 ) ;
#18228 = ORIENTED_EDGE ( 'NONE', *, *, #21550, .F. ) ;
#18229 = DIRECTION ( 'NONE',  ( 0.000000000000000000, 0.000000000000000000, 1.000000000000000000 ) ) ;
#18230 = CARTESIAN_POINT ( 'NONE',  ( 52.72106816583844591, 13.02818770551464489, 16.17458954617363531 ) ) ;
#18231 = EDGE_CURVE ( 'NONE', #15133, #2520, #9936, .T. ) ;
#18232 = CARTESIAN_POINT ( 'NONE',  ( -69.45000000109247651, 12.06698730000000097, 14.99999999999999645 ) ) ;
#18233 = VECTOR ( 'NONE', #16822, 1000.000000000000000 ) ;
#18234 = CARTESIAN_POINT ( 'NONE',  ( -68.40000000109246514, 7.933012699999995476, 15.85617417291294196 ) ) ;
#18235 = CARTESIAN_POINT ( 'NONE',  ( -1.799999999999996048, 0.000000000000000000, 0.000000000000000000 ) ) ;
#18236 = CARTESIAN_POINT ( 'NONE',  ( 4.000000000000000888, 1.656854249492381248, 10.68750000273119483 ) ) ;
#18237 = CARTESIAN_POINT ( 'NONE',  ( 53.34375000000000000, 8.757359312880723223, 18.00000000000000355 ) ) ;
#18238 = DIRECTION ( 'NONE',  ( 0.000000000000000000, 0.000000000000000000, -1.000000000000000000 ) ) ;
#18239 = CARTESIAN_POINT ( 'NONE',  ( 51.46875000000000000, 6.999999999999992895, 13.75735931288071967 ) ) ;
#18240 = CARTESIAN_POINT ( 'NONE',  ( -68.09999999999999432, 9.999999999999998224, 12.49999999999999289 ) ) ;
#18241 = AXIS2_PLACEMENT_3D ( 'NONE', #9084, #13036, #3778 ) ;
#18242 = ORIENTED_EDGE ( 'NONE', *, *, #4398, .T. ) ;
#18243 = CARTESIAN_POINT ( 'NONE',  ( 70.20000000218495018, 9.999999999999998224, 17.49999999999999645 ) ) ;
#18244 = LINE ( 'NONE', #10968, #15498 ) ;
#18245 = ORIENTED_EDGE ( 'NONE', *, *, #6725, .T. ) ;
#18246 = CARTESIAN_POINT ( 'NONE',  ( 55.68750000000000000, 9.999999999999989342, 11.99999999999999467 ) ) ;
#18247 =( NAMED_UNIT ( * ) PLANE_ANGLE_UNIT ( ) SI_UNIT ( $, .RADIAN. ) );
#18248 = CARTESIAN_POINT ( 'NONE',  ( -2.449293598294706907E-16, 4.000000000000000000, -3.824999997268811569 ) ) ;
#18249 = CARTESIAN_POINT ( 'NONE',  ( -72.15000000109247935, 9.999999999999998224, 17.49999999999999645 ) ) ;
#18250 = VERTEX_POINT ( 'NONE', #10058 ) ;
#18251 = CARTESIAN_POINT ( 'NONE',  ( -3.999999999999998224, -1.656854249492383246, 16.06250000000001066 ) ) ;
#18252 = CARTESIAN_POINT ( 'NONE',  ( 60.00000000000000711, 15.00000000000000000, 10.00000000000007105 ) ) ;
#18253 = DIRECTION ( 'NONE',  ( 0.000000000000000000, 0.000000000000000000, 1.000000000000000000 ) ) ;
#18254 = VERTEX_POINT ( 'NONE', #8013 ) ;
#18255 =( LENGTH_UNIT ( ) NAMED_UNIT ( * ) SI_UNIT ( .MILLI., .METRE. ) );
#18256 = VECTOR ( 'NONE', #19431, 1000.000000000000000 ) ;
#18257 = ADVANCED_FACE ( 'NONE', ( #4520 ), #8651, .T. ) ;
#18258 = DIRECTION ( 'NONE',  ( 0.000000000000000000, 0.000000000000000000, -1.000000000000000000 ) ) ;
#18259 = ADVANCED_FACE ( 'NONE', ( #21255 ), #21141, .T. ) ;
#18260 = CARTESIAN_POINT ( 'NONE',  ( 2.445694354108820079, 2.445694354108820523, 0.6125000013655953479 ) ) ;
#18261 = CIRCLE ( 'NONE', #1040, 11.00000000000000000 ) ;
#18262 = CARTESIAN_POINT ( 'NONE',  ( 69.74999999999998579, 11.03553390593273598, 12.49999999999999289 ) ) ;
#18263 = ADVANCED_FACE ( 'NONE', ( #17348 ), #10587, .T. ) ;
#18264 = CARTESIAN_POINT ( 'NONE',  ( 4.999999999999999112, 2.223716399045689407, -8.461683424509292450 ) ) ;
#18265 = CARTESIAN_POINT ( 'NONE',  ( -5.555405146766190683, -9.000000000000005329, 5.000000000000079936 ) ) ;
#18266 = CARTESIAN_POINT ( 'NONE',  ( 51.40856816583843880, 13.97181229448534978, 13.27509460956196641 ) ) ;
#18267 = CARTESIAN_POINT ( 'NONE',  ( 3.458734125000000326, 4.235727675282971730E-16, -1.762499998634403209 ) ) ;
#18268 = DIRECTION ( 'NONE',  ( -0.3420201433256622181, 0.9396926207859106484, 1.232595164407828100E-31 ) ) ;
#18269 = CARTESIAN_POINT ( 'NONE',  ( -4.000000000000000000, 0.000000000000000000, 0.3000000000000016542 ) ) ;
#18270 = AXIS2_PLACEMENT_3D ( 'NONE', #3119, #12613, #19753 ) ;
#18271 = DIRECTION ( 'NONE',  ( -1.000000000000000000, -0.000000000000000000, 0.000000000000000000 ) ) ;
#18272 = VERTEX_POINT ( 'NONE', #22716 ) ;
#18273 = CARTESIAN_POINT ( 'NONE',  ( 0.000000000000000000, 0.000000000000000000, 20.00000000000001066 ) ) ;
#18274 = CARTESIAN_POINT ( 'NONE',  ( -65.00000000000000000, 9.999999999999998224, 17.49999999999999645 ) ) ;
#18275 = DIRECTION ( 'NONE',  ( 0.000000000000000000, -1.000000000000000000, -0.000000000000000000 ) ) ;
#18276 = ORIENTED_EDGE ( 'NONE', *, *, #16541, .T. ) ;
#18277 = VECTOR ( 'NONE', #11340, 1000.000000000000000 ) ;
#18278 = ORIENTED_EDGE ( 'NONE', *, *, #18404, .T. ) ;
#18279 = VECTOR ( 'NONE', #23414, 1000.000000000000000 ) ;
#18280 = PRESENTATION_STYLE_ASSIGNMENT (( #20300 ) ) ;
#18281 =( GEOMETRIC_REPRESENTATION_CONTEXT ( 3 ) GLOBAL_UNCERTAINTY_ASSIGNED_CONTEXT ( ( #666 ) ) GLOBAL_UNIT_ASSIGNED_CONTEXT ( ( #20509, #16941, #22553 ) ) REPRESENTATION_CONTEXT ( 'NONE', 'WORKASPACE' ) );
#18282 = ADVANCED_FACE ( 'NONE', ( #19355 ), #2594, .F. ) ;
#18283 = VERTEX_POINT ( 'NONE', #12208 ) ;
#18284 = CARTESIAN_POINT ( 'NONE',  ( 53.81250000000000711, 14.00000000000000000, 14.99999999999997691 ) ) ;
#18285 = ORIENTED_EDGE ( 'NONE', *, *, #19407, .T. ) ;
#18286 = CARTESIAN_POINT ( 'NONE',  ( 5.000000000000000000, 0.000000000000000000, 1.000000000000000000 ) ) ;
#18287 = ORIENTED_EDGE ( 'NONE', *, *, #1294, .T. ) ;
#18288 = CARTESIAN_POINT ( 'NONE',  ( 57.12731816583843170, 12.87654654797634102, 17.78030770151602979 ) ) ;
#18289 = AXIS2_PLACEMENT_3D ( 'NONE', #20261, #2054, #11442 ) ;
#18290 = EDGE_CURVE ( 'NONE', #5128, #19003, #22381, .T. ) ;
#18291 = CARTESIAN_POINT ( 'NONE',  ( 71.75000000109248788, 11.46158073645647235, 13.53841926354352232 ) ) ;
#18292 = AXIS2_PLACEMENT_3D ( 'NONE', #6730, #12024, #17747 ) ;
#18293 = CARTESIAN_POINT ( 'NONE',  ( 0.000000000000000000, -1.178949249685218748, -2.041999999999998039 ) ) ;
#18294 = LINE ( 'NONE', #1878, #22080 ) ;
#18295 = DIRECTION ( 'NONE',  ( 1.224646799147353207E-16, 1.000000000000000000, 0.000000000000000000 ) ) ;
#18296 = EDGE_CURVE ( 'NONE', #12128, #6311, #3648, .T. ) ;
#18297 = ORIENTED_EDGE ( 'NONE', *, *, #6457, .T. ) ;
#18298 = CARTESIAN_POINT ( 'NONE',  ( 2.828427124746191179, 2.828427124746190291, 17.75000000273119483 ) ) ;
#18299 = ADVANCED_FACE ( 'NONE', ( #8138 ), #19479, .T. ) ;
#18300 = AXIS2_PLACEMENT_3D ( 'NONE', #16494, #23672, #12802 ) ;
#18301 = DIRECTION ( 'NONE',  ( 0.000000000000000000, 0.000000000000000000, -1.000000000000000000 ) ) ;
#18302 = STYLED_ITEM ( 'NONE', ( #7961 ), #23316 ) ;
#18303 = CARTESIAN_POINT ( 'NONE',  ( 53.68518183416157541, 10.06805114094561659, 10.99999999999999645 ) ) ;
#18304 = CARTESIAN_POINT ( 'NONE',  ( -2.117863837641482907E-16, 3.458734125000000770, -3.273533850472710061 ) ) ;
#18305 = LINE ( 'NONE', #1887, #11285 ) ;
#18306 = CARTESIAN_POINT ( 'NONE',  ( -67.99999999999998579, 8.232233047033629347, 13.23223304703362402 ) ) ;
#18307 = DIRECTION ( 'NONE',  ( -2.465190328815656418E-32, -0.3420201433256690460, 0.9396926207859083169 ) ) ;
#18308 = ORIENTED_EDGE ( 'NONE', *, *, #2192, .F. ) ;
#18309 = LINE ( 'NONE', #1539, #5873 ) ;
#18310 = CARTESIAN_POINT ( 'NONE',  ( 51.18750000000000711, 9.999999999999989342, 11.99999999999999467 ) ) ;
#18311 = DIRECTION ( 'NONE',  ( 1.000000000000000000, 0.000000000000000000, -1.224646799147353207E-16 ) ) ;
#18312 = AXIS2_PLACEMENT_3D ( 'NONE', #13115, #7721, #9393 ) ;
#18313 = ORIENTED_EDGE ( 'NONE', *, *, #22666, .F. ) ;
#18314 = VECTOR ( 'NONE', #880, 1000.000000000000000 ) ;
#18315 = CYLINDRICAL_SURFACE ( 'NONE', #13225, 4.000000000000000000 ) ;
#18316 = CARTESIAN_POINT ( 'NONE',  ( -3.458734125000000326, 0.000000000000000000, -3.262499998634404541 ) ) ;
#18317 = FACE_OUTER_BOUND ( 'NONE', #1692, .T. ) ;
#18318 = VERTEX_POINT ( 'NONE', #20906 ) ;
#18319 = LINE ( 'NONE', #14751, #9167 ) ;
#18320 = ORIENTED_EDGE ( 'NONE', *, *, #23560, .F. ) ;
#18321 = CARTESIAN_POINT ( 'NONE',  ( 1.520000000000000462, 0.000000000000000000, 0.000000000000000000 ) ) ;
#18322 = VECTOR ( 'NONE', #5861, 1000.000000000000000 ) ;
#18323 = EDGE_CURVE ( 'NONE', #6488, #2752, #17588, .T. ) ;
#18324 = CARTESIAN_POINT ( 'NONE',  ( 2.828427124746191179, 2.828427124746190291, 18.62500000000001066 ) ) ;
#18325 = CARTESIAN_POINT ( 'NONE',  ( 0.000000000000000000, 0.000000000000000000, -3.700000000000000178 ) ) ;
#18326 = CYLINDRICAL_SURFACE ( 'NONE', #11081, 2.649999999999999467 ) ;
#18327 = EDGE_CURVE ( 'NONE', #16821, #12663, #7112, .T. ) ;
#18329 = EDGE_CURVE ( 'NONE', #16373, #3506, #7506, .T. ) ;
#18328 = CIRCLE ( 'NONE', #14528, 2.649999999999989253 ) ;
#18330 = EDGE_LOOP ( 'NONE', ( #19453, #22691 ) ) ;
#18331 = ADVANCED_FACE ( 'NONE', ( #6447 ), #8372, .F. ) ;
#18332 = CIRCLE ( 'NONE', #7650, 5.000000000000000888 ) ;
#18333 = CARTESIAN_POINT ( 'NONE',  ( -67.79999999999999716, 8.232233047033627571, 16.76776695296636532 ) ) ;
#18334 = CARTESIAN_POINT ( 'NONE',  ( 66.30000000218494449, 8.232233047033627571, 16.76776695296636532 ) ) ;
#18335 = CARTESIAN_POINT ( 'NONE',  ( 67.25000000109247367, 9.999999999999998224, 17.06698730000000097 ) ) ;
#18336 = CARTESIAN_POINT ( 'NONE',  ( 1.025207404391860050E-15, 3.458734125000000326, 18.18750000136560274 ) ) ;
#18337 = CARTESIAN_POINT ( 'NONE',  ( 4.197393957002303999, 7.772902908466098641E-14, -3.503767560748929810 ) ) ;
#18338 = PRESENTATION_LAYER_ASSIGNMENT (  '', '', ( #8030 ) ) ;
#18339 = MECHANICAL_DESIGN_GEOMETRIC_PRESENTATION_REPRESENTATION (  '', ( #8032 ), #6848 ) ;
#18340 = CARTESIAN_POINT ( 'NONE',  ( -1.656854249492381248, -3.999999999999999112, 4.487499999999999822 ) ) ;
#18341 = CARTESIAN_POINT ( 'NONE',  ( 67.00000000218494733, 9.999999999999998224, 17.49999999999999645 ) ) ;
#18342 = CARTESIAN_POINT ( 'NONE',  ( 1.872352939448454495E-15, -3.458734125000000326, 14.68750000136560452 ) ) ;
#18343 = LINE ( 'NONE', #1923, #8074 ) ;
#18344 = ORIENTED_EDGE ( 'NONE', *, *, #11430, .T. ) ;
#18345 = CARTESIAN_POINT ( 'NONE',  ( -70.40000000109249356, 10.85617417291294551, 17.06698730000000097 ) ) ;
#18346 = EDGE_LOOP ( 'NONE', ( #9411, #19046, #21978, #20686 ) ) ;
#18347 = CARTESIAN_POINT ( 'NONE',  ( 54.24768183416157541, 7.123453452023678523, 17.78030770151605822 ) ) ;
#18348 = CARTESIAN_POINT ( 'NONE',  ( -71.60000000109246798, 7.933012699999995476, 15.85617417291294196 ) ) ;
#18349 = SHAPE_DEFINITION_REPRESENTATION ( #7618, #18175 ) ;
#18350 = CONICAL_SURFACE ( 'NONE', #8041, 6.500000000000000888, 1.047197551196596521 ) ;
#18351 = CARTESIAN_POINT ( 'NONE',  ( 4.000000000000001776, -1.656854249492379694, 17.43750000000001066 ) ) ;
#18352 = ORIENTED_EDGE ( 'NONE', *, *, #20777, .F. ) ;
#18353 = ORIENTED_EDGE ( 'NONE', *, *, #23667, .F. ) ;
#18354 = CARTESIAN_POINT ( 'NONE',  ( -3.999999999999999112, 0.000000000000000000, 15.00000000000001066 ) ) ;
#18355 = CARTESIAN_POINT ( 'NONE',  ( 52.43981816583844591, 10.06805114094563791, 17.99999999999999645 ) ) ;
#18356 = CARTESIAN_POINT ( 'NONE',  ( -71.35000000109246798, 8.538419263543522320, 16.46158073645647235 ) ) ;
#18357 = MECHANICAL_DESIGN_GEOMETRIC_PRESENTATION_REPRESENTATION (  '', ( #6504 ), #1129 ) ;
#18358 = EDGE_CURVE ( 'NONE', #3528, #20275, #4378, .T. ) ;
#18359 = CARTESIAN_POINT ( 'NONE',  ( -69.65000000109246514, 12.06698730000000097, 14.99999999999999645 ) ) ;
#18360 = CARTESIAN_POINT ( 'NONE',  ( 3.458734125000002546, -1.432654583217639610, 13.12500000136560629 ) ) ;
#18361 = FACE_OUTER_BOUND ( 'NONE', #22877, .T. ) ;
#18362 = CARTESIAN_POINT ( 'NONE',  ( 60.99768183416157541, 12.16943976678977535, 12.92679907967048614 ) ) ;
#18363 = DIRECTION ( 'NONE',  ( -1.000000000000000000, -0.000000000000000000, -0.000000000000000000 ) ) ;
#18364 = AXIS2_PLACEMENT_3D ( 'NONE', #8187, #15500, #20847 ) ;
#18365 = CARTESIAN_POINT ( 'NONE',  ( 54.84375000000000000, 8.757359312880723223, 18.00000000000000355 ) ) ;
#18366 = CARTESIAN_POINT ( 'NONE',  ( 9.920644283265380691E-16, 4.000000000000000000, 16.87500000273119838 ) ) ;
#18367 = CARTESIAN_POINT ( 'NONE',  ( -69.00000000218494733, 9.999999999999998224, 12.49999999999999289 ) ) ;
#18368 = AXIS2_PLACEMENT_3D ( 'NONE', #6330, #11977, #1036 ) ;
#18369 = ORIENTED_EDGE ( 'NONE', *, *, #13492, .T. ) ;
#18370 = CARTESIAN_POINT ( 'NONE',  ( -3.270501301980698550, -1.125461230421587633, 2.040000000000001812 ) ) ;
#18371 = VERTEX_POINT ( 'NONE', #20795 ) ;
#18372 = CARTESIAN_POINT ( 'NONE',  ( 53.06250000000000711, 6.999999999999997335, 15.00000000000000533 ) ) ;
#18373 = CIRCLE ( 'NONE', #11522, 4.000000000000000000 ) ;
#18374 = CARTESIAN_POINT ( 'NONE',  ( -2.828427124746190291, 2.828427124746190291, -2.699999997268812457 ) ) ;
#18375 = DIRECTION ( 'NONE',  ( 1.000000000000000000, 0.000000000000000000, 0.000000000000000000 ) ) ;
#18376 = VERTEX_POINT ( 'NONE', #6680 ) ;
#18377 = CARTESIAN_POINT ( 'NONE',  ( 9.920644283265380691E-16, 4.000000000000000000, 18.75000000000001066 ) ) ;
#18378 = CARTESIAN_POINT ( 'NONE',  ( 45.00000000000000000, 15.00000000000001954, 10.00000000000008882 ) ) ;
#18379 = CARTESIAN_POINT ( 'NONE',  ( 69.20000000000000284, 11.76776695296636888, 16.76776695296636532 ) ) ;
#18380 = VERTEX_POINT ( 'NONE', #11739 ) ;
#18381 = CYLINDRICAL_SURFACE ( 'NONE', #9189, 5.000000000000001776 ) ;
#18382 = DIRECTION ( 'NONE',  ( 0.000000000000000000, 0.000000000000000000, 1.000000000000000000 ) ) ;
#18383 = CARTESIAN_POINT ( 'NONE',  ( 3.458734125000001214, -1.432654583217639610, 0.4250000013655961251 ) ) ;
#18384 = CIRCLE ( 'NONE', #21817, 2.500000000000007550 ) ;
#18385 = CARTESIAN_POINT ( 'NONE',  ( 68.20000000000000284, 11.76776695296636888, 13.23223304703362579 ) ) ;
#18386 = DIRECTION ( 'NONE',  ( -1.000000000000000000, 0.000000000000000000, 0.000000000000000000 ) ) ;
#18387 = DIRECTION ( 'NONE',  ( 1.000000000000000000, 0.000000000000000000, 0.000000000000000000 ) ) ;
#18388 = CARTESIAN_POINT ( 'NONE',  ( 54.68981816583844591, 9.931948859054346102, 10.99999999999999467 ) ) ;
#18389 = CARTESIAN_POINT ( 'NONE',  ( 3.458734125000000326, 1.432654583217640498, 1.300000001365597235 ) ) ;
#18390 = CARTESIAN_POINT ( 'NONE',  ( -3.458734124999998993, -1.432654583217642497, 13.75000000136560452 ) ) ;
#18391 = CARTESIAN_POINT ( 'NONE',  ( -1.489200000000000079, 0.000000000000000000, 0.000000000000000000 ) ) ;
#18392 = PLANE ( 'NONE',  #5935 ) ;
#18393 = EDGE_CURVE ( 'NONE', #14895, #3750, #10187, .T. ) ;
#18394 = DIRECTION ( 'NONE',  ( 1.000000000000000000, 7.703719777548943412E-32, 0.000000000000000000 ) ) ;
#18395 = ORIENTED_EDGE ( 'NONE', *, *, #5127, .F. ) ;
#18396 = CARTESIAN_POINT ( 'NONE',  ( 6.500000000000000000, -3.142418015001832376, -3.295638806298775147 ) ) ;
#18397 = LINE ( 'NONE', #20294, #20194 ) ;
#18398 = FACE_OUTER_BOUND ( 'NONE', #1240, .T. ) ;
#18399 = AXIS2_PLACEMENT_3D ( 'NONE', #17495, #22747, #6359 ) ;
#18400 = ORIENTED_EDGE ( 'NONE', *, *, #17438, .T. ) ;
#18401 = EDGE_LOOP ( 'NONE', ( #2356, #490, #21213, #23159 ) ) ;
#18402 = LINE ( 'NONE', #9562, #2578 ) ;
#18403 = ORIENTED_EDGE ( 'NONE', *, *, #15201, .T. ) ;
#18404 = EDGE_CURVE ( 'NONE', #18050, #5914, #12441, .T. ) ;
#18405 = CARTESIAN_POINT ( 'NONE',  ( 58.21875000000000711, 14.00000000000001066, 16.65685424949235482 ) ) ;
#18406 = EDGE_LOOP ( 'NONE', ( #16937, #432, #705, #15552 ) ) ;
#18407 = DIRECTION ( 'NONE',  ( 0.000000000000000000, 0.000000000000000000, 1.000000000000000000 ) ) ;
#18408 = EDGE_LOOP ( 'NONE', ( #539, #6548, #1276, #19363 ) ) ;
#18409 = CARTESIAN_POINT ( 'NONE',  ( 56.28356816583844591, 8.275094609561968184, 11.02818770551464667 ) ) ;
#18410 = CARTESIAN_POINT ( 'NONE',  ( 71.70000000109247651, 10.85617417291294551, 12.93301269999999370 ) ) ;
#18411 = CARTESIAN_POINT ( 'NONE',  ( 10.97149113033275114, -11.25000000000000355, 5.000000000000079936 ) ) ;
#18412 = CARTESIAN_POINT ( 'NONE',  ( 71.45000000109247651, 9.999999999999998224, 17.06698730000000097 ) ) ;
#18413 = ORIENTED_EDGE ( 'NONE', *, *, #21650, .T. ) ;
#18414 = CARTESIAN_POINT ( 'NONE',  ( -1.656854249492379250, 4.000000000000000000, 15.93750000273119838 ) ) ;
#18415 = DIRECTION ( 'NONE',  ( 1.000000000000000000, 0.000000000000000000, 0.000000000000000000 ) ) ;
#18416 = CARTESIAN_POINT ( 'NONE',  ( 59.71875000000000711, 14.00000000000000888, 16.65685424949235482 ) ) ;
#18417 = DIRECTION ( 'NONE',  ( 0.000000000000000000, 0.000000000000000000, -1.000000000000000000 ) ) ;
#18418 = DIRECTION ( 'NONE',  ( 1.000000000000000000, 0.000000000000000000, -0.000000000000000000 ) ) ;
#18419 = DIRECTION ( 'NONE',  ( 1.000000000000000000, 0.000000000000000000, 0.000000000000000000 ) ) ;
#18420 = EDGE_CURVE ( 'NONE', #4822, #10125, #9038, .T. ) ;
#18421 = CARTESIAN_POINT ( 'NONE',  ( 4.000000000000000000, 1.680228229147133767, -3.316631783032546021 ) ) ;
#18422 = VERTEX_POINT ( 'NONE', #23432 ) ;
#18423 = DIRECTION ( 'NONE',  ( 0.8660254037844374864, -0.5000000000000018874, 0.000000000000000000 ) ) ;
#18424 = EDGE_CURVE ( 'NONE', #660, #17422, #8600, .T. ) ;
#18425 = CARTESIAN_POINT ( 'NONE',  ( 54.00000000000000711, 12.12132034355963484, 12.87867965644034740 ) ) ;
#18426 = DIRECTION ( 'NONE',  ( 0.000000000000000000, 0.000000000000000000, -1.000000000000000000 ) ) ;
#18427 = ORIENTED_EDGE ( 'NONE', *, *, #15505, .T. ) ;
#18428 = DIRECTION ( 'NONE',  ( 0.000000000000000000, 0.000000000000000000, 1.000000000000000000 ) ) ;
#18429 = CARTESIAN_POINT ( 'NONE',  ( 1.656854249492381470, 4.000000000000000000, 14.81250000273119838 ) ) ;
#18430 = CARTESIAN_POINT ( 'NONE',  ( 1.411581201560190495E-15, 4.862606272033091592, -3.745885042887436622 ) ) ;
#18431 = EDGE_CURVE ( 'NONE', #13541, #7101, #15906, .T. ) ;
#18432 = LINE ( 'NONE', #5745, #11405 ) ;
#18433 = ORIENTED_EDGE ( 'NONE', *, *, #216, .F. ) ;
#18434 = CARTESIAN_POINT ( 'NONE',  ( 14.99999999999995559, -15.00000000000000000, -50.00000000000000000 ) ) ;
#18435 = VERTEX_POINT ( 'NONE', #5349 ) ;
#18436 = ADVANCED_FACE ( 'NONE', ( #20052 ), #21737, .F. ) ;
#18437 = LINE ( 'NONE', #16532, #20573 ) ;
#18438 = CARTESIAN_POINT ( 'NONE',  ( 1.656854249492384135, -3.999999999999999112, 16.31250000000001066 ) ) ;
#18439 = CARTESIAN_POINT ( 'NONE',  ( 4.999999999999999112, 0.000000000000000000, 0.000000000000000000 ) ) ;
#18440 = FACE_BOUND ( 'NONE', #8998, .T. ) ;
#18441 = CARTESIAN_POINT ( 'NONE',  ( 1.656854249492381470, 4.000000000000000000, 17.81250000273119483 ) ) ;
#18442 = ORIENTED_EDGE ( 'NONE', *, *, #4343, .T. ) ;
#18443 = CARTESIAN_POINT ( 'NONE',  ( -68.45000000000000284, 11.03553390593273598, 17.50000000000000355 ) ) ;
#18444 = EDGE_CURVE ( 'NONE', #1719, #1746, #6795, .T. ) ;
#18445 = AXIS2_PLACEMENT_3D ( 'NONE', #19712, #12445, #15691 ) ;
#18446 = DIRECTION ( 'NONE',  ( -1.000000000000000000, -0.000000000000000000, -0.000000000000000000 ) ) ;
#18447 = CARTESIAN_POINT ( 'NONE',  ( 66.65000000109247935, 7.933012699999995476, 14.99999999999999645 ) ) ;
#18448 = CARTESIAN_POINT ( 'NONE',  ( -3.458734124999998993, 1.432654583217640276, 16.37500000136560629 ) ) ;
#18449 = CARTESIAN_POINT ( 'NONE',  ( 0.000000000000000000, 0.000000000000000000, 19.04999999999996874 ) ) ;
#18450 = CARTESIAN_POINT ( 'NONE',  ( 4.999999999999999112, 9.915734732513218574, 4.762163868918307230 ) ) ;
#18451 =( BOUNDED_CURVE ( )  B_SPLINE_CURVE ( 2, ( #1440, #14292, #4697, #19295, #5165, #10711, #8544, #2886, #15746 ),
 .UNSPECIFIED., .F., .F. ) 
 B_SPLINE_CURVE_WITH_KNOTS ( ( 3, 2, 2, 2, 3 ),
 ( 0.6875000000000001110, 0.7031250000000000000, 0.7187500000000000000, 0.7343749999999998890, 0.7499999999999997780 ),
 .UNSPECIFIED. ) 
 CURVE ( )  GEOMETRIC_REPRESENTATION_ITEM ( )  RATIONAL_B_SPLINE_CURVE ( ( 0.9999999999999994449, 0.9238795325112872936, 1.000000000000000000, 0.9238795325112867385, 1.000000000000000000, 0.9238795325112867385, 1.000000000000000000, 0.9238795325112878487, 0.9999999999999988898 ) ) 
 REPRESENTATION_ITEM ( '' )  );
#18452 = CARTESIAN_POINT ( 'NONE',  ( 1.432654583217642275, -3.458734124999999882, -2.699999998634404541 ) ) ;
#18453 = ADVANCED_FACE ( 'NONE', ( #21857 ), #19947, .T. ) ;
#18454 = CARTESIAN_POINT ( 'NONE',  ( 2.000000000000001776, 0.000000000000000000, 6.543750000000017053 ) ) ;
#18455 = CARTESIAN_POINT ( 'NONE',  ( 1.432654583217641164, 3.458734125000000326, 13.12500000136560274 ) ) ;
#18456 = CARTESIAN_POINT ( 'NONE',  ( -67.20000000218495018, 7.499999999999996447, 14.99999999999999645 ) ) ;
#18457 = ORIENTED_EDGE ( 'NONE', *, *, #18863, .F. ) ;
#18458 = CARTESIAN_POINT ( 'NONE',  ( -69.40000000109249356, 12.06698729999999919, 14.14382582708705094 ) ) ;
#18459 = ORIENTED_EDGE ( 'NONE', *, *, #12655, .T. ) ;
#18460 = CARTESIAN_POINT ( 'NONE',  ( 54.52893183416158962, 11.58880310854676132, 19.02818770551463956 ) ) ;
#18461 = CARTESIAN_POINT ( 'NONE',  ( -69.65000000109246514, 12.06698730000000097, 14.99999999999999645 ) ) ;
#18462 = CONTEXT_DEPENDENT_SHAPE_REPRESENTATION ( #22761, #9538 ) ;
#18463 = EDGE_CURVE ( 'NONE', #13481, #17633, #15164, .T. ) ;
#18464 = CARTESIAN_POINT ( 'NONE',  ( 1.971781867644420635E-15, -4.000000000000000000, 17.25000000000001066 ) ) ;
#18465 = ORIENTED_EDGE ( 'NONE', *, *, #8231, .F. ) ;
#18466 = EDGE_CURVE ( 'NONE', #2990, #22965, #17700, .T. ) ;
#18467 = VERTEX_POINT ( 'NONE', #19591 ) ;
#18468 = CARTESIAN_POINT ( 'NONE',  ( 71.29999999999998295, 9.999999999999998224, 12.49999999999999289 ) ) ;
#18469 = CARTESIAN_POINT ( 'NONE',  ( 54.09375000000000711, 11.24264068711927322, 11.99999999999998934 ) ) ;
#18470 = CARTESIAN_POINT ( 'NONE',  ( -71.05000000109247082, 12.06698730000000097, 14.99999999999999645 ) ) ;
#18471 = CARTESIAN_POINT ( 'NONE',  ( -69.55000000109247082, 11.46158073645647235, 13.53841926354352232 ) ) ;
#18472 = CARTESIAN_POINT ( 'NONE',  ( 3.458734125000001658, 4.235727675282972223E-16, 12.18750000136560629 ) ) ;
#18473 = CARTESIAN_POINT ( 'NONE',  ( -6.170261003233799890, -9.000000000000005329, 5.000000000000079936 ) ) ;
#18474 = CARTESIAN_POINT ( 'NONE',  ( 52.50000000000000711, 12.12132034355963484, 12.87867965644034740 ) ) ;
#18475 = DIRECTION ( 'NONE',  ( 1.000000000000000000, 0.000000000000000000, 0.000000000000000000 ) ) ;
#18476 = CARTESIAN_POINT ( 'NONE',  ( 52.21875000000002842, 13.00000000000000711, 16.24264068711927322 ) ) ;
#18477 = CARTESIAN_POINT ( 'NONE',  ( 1.971781867644420635E-15, -4.000000000000000000, 16.37500000273119838 ) ) ;
#18478 = CARTESIAN_POINT ( 'NONE',  ( 68.59999999999999432, 8.232233047033627571, 16.76776695296636532 ) ) ;
#18479 = VECTOR ( 'NONE', #890, 1000.000000000000000 ) ;
#18480 = VERTEX_POINT ( 'NONE', #17927 ) ;
#18481 = CARTESIAN_POINT ( 'NONE',  ( -71.50000000218496155, 11.76776695296636888, 13.23223304703362579 ) ) ;
#18482 = VERTEX_POINT ( 'NONE', #5000 ) ;
#18483 = CARTESIAN_POINT ( 'NONE',  ( 57.09375000000000711, 11.24264068711927322, 11.99999999999998934 ) ) ;
#18484 = CARTESIAN_POINT ( 'NONE',  ( 4.000000000000000888, -1.656854249492379694, -2.137499997268812013 ) ) ;
#18485 = VECTOR ( 'NONE', #1318, 1000.000000000000000 ) ;
#18486 = EDGE_CURVE ( 'NONE', #2584, #6221, #9800, .T. ) ;
#18487 = CARTESIAN_POINT ( 'NONE',  ( 72.50000000000000000, 9.999999999999998224, 17.49999999999999645 ) ) ;
#18488 = ORIENTED_EDGE ( 'NONE', *, *, #7967, .F. ) ;
#18489 = CARTESIAN_POINT ( 'NONE',  ( -1.656854249492379250, 4.000000000000000000, 13.81250000000001066 ) ) ;
#18490 = EDGE_CURVE ( 'NONE', #3871, #6195, #1379, .T. ) ;
#18491 = CARTESIAN_POINT ( 'NONE',  ( -4.000000000000000000, 0.000000000000000000, -2.699999999999999289 ) ) ;
#18492 = CARTESIAN_POINT ( 'NONE',  ( 2.500000000000000000, 2.357898499370431722, -2.818925648462311528E-15 ) ) ;
#18493 = EDGE_LOOP ( 'NONE', ( #21315, #8839, #8758, #20178 ) ) ;
#18494 = CARTESIAN_POINT ( 'NONE',  ( -7.878064769667250999, -11.25000000000000355, 10.00000000000008882 ) ) ;
#18495 = DIRECTION ( 'NONE',  ( -1.000000000000000000, 0.000000000000000000, -0.000000000000000000 ) ) ;
#18496 = CARTESIAN_POINT ( 'NONE',  ( 69.45000000000000284, 7.499999999999995559, 16.03553390593273420 ) ) ;
#18497 = LINE ( 'NONE', #22072, #4345 ) ;
#18498 = CARTESIAN_POINT ( 'NONE',  ( 2.503708927703406609E-30, 1.503597262882131219E-46, -0.8737698471611414774 ) ) ;
#18499 = CARTESIAN_POINT ( 'NONE',  ( 54.40856816583843880, 13.97181229448534978, 13.27509460956196641 ) ) ;
#18500 = CARTESIAN_POINT ( 'NONE',  ( 3.458734125000000770, -1.432654583217639610, 0.1750000013655959585 ) ) ;
#18501 = CARTESIAN_POINT ( 'NONE',  ( 3.458734125000002546, -1.432654583217639610, 14.12500000136560452 ) ) ;
#18502 = CARTESIAN_POINT ( 'NONE',  ( 69.00000000218494733, 9.999999999999998224, 12.49999999999999289 ) ) ;
#18503 = CARTESIAN_POINT ( 'NONE',  ( -70.95000000109247651, 8.538419263543524096, 13.53841926354352054 ) ) ;
#18504 = CARTESIAN_POINT ( 'NONE',  ( 0.000000000000000000, 0.000000000000000000, 8.749000000000002331 ) ) ;
#18505 = ORIENTED_EDGE ( 'NONE', *, *, #4692, .F. ) ;
#18506 = DIRECTION ( 'NONE',  ( 0.000000000000000000, 5.754033390038007439E-16, 1.000000000000000000 ) ) ;
#18507 = CARTESIAN_POINT ( 'NONE',  ( 35.28529930323381336, -9.000000000000003553, 5.000000000000079936 ) ) ;
#18508 = CARTESIAN_POINT ( 'NONE',  ( -70.09999999999999432, 9.999999999999998224, 17.49999999999999645 ) ) ;
#18509 = VERTEX_POINT ( 'NONE', #23551 ) ;
#18510 = ORIENTED_EDGE ( 'NONE', *, *, #8171, .F. ) ;
#18511 = CARTESIAN_POINT ( 'NONE',  ( 72.50000000000000000, 9.999999999999998224, 17.49999999999999645 ) ) ;
#18512 = VECTOR ( 'NONE', #15394, 1000.000000000000000 ) ;
#18513 = CARTESIAN_POINT ( 'NONE',  ( 54.84375000000000711, 8.343145750507636293, 19.00000000000000000 ) ) ;
#18514 = EDGE_LOOP ( 'NONE', ( #3107, #4652, #14608, #13293 ) ) ;
#18515 = LINE ( 'NONE', #3556, #14901 ) ;
#18516 = ORIENTED_EDGE ( 'NONE', *, *, #20734, .F. ) ;
#18517 = CARTESIAN_POINT ( 'NONE',  ( 55.25231816583843170, 7.219692298483957771, 17.87654654797633924 ) ) ;
#18518 = AXIS2_PLACEMENT_3D ( 'NONE', #5966, #16399, #92 ) ;
#18519 = CARTESIAN_POINT ( 'NONE',  ( 70.25000000109247367, 12.06698730000000097, 14.99999999999999645 ) ) ;
#18520 = EDGE_CURVE ( 'NONE', #20740, #9225, #4427, .T. ) ;
#18521 = VECTOR ( 'NONE', #21318, 1000.000000000000000 ) ;
#18522 = FACE_OUTER_BOUND ( 'NONE', #20182, .T. ) ;
#18523 = CARTESIAN_POINT ( 'NONE',  ( 70.45000000109247651, 12.06698730000000097, 14.99999999999999645 ) ) ;
#18524 = ORIENTED_EDGE ( 'NONE', *, *, #11998, .T. ) ;
#18525 = CARTESIAN_POINT ( 'NONE',  ( -1.656854249492379250, 4.000000000000000000, 16.93750000273119838 ) ) ;
#18526 = CARTESIAN_POINT ( 'NONE',  ( 60.00000000000000711, -15.00000000000000000, 10.00000000000007105 ) ) ;
#18527 = CARTESIAN_POINT ( 'NONE',  ( 55.09143183416158962, 11.72490539043799984, 11.02818770551463246 ) ) ;
#18528 = CARTESIAN_POINT ( 'NONE',  ( -2.117863837641485618E-16, 3.458734125000000770, -3.262499998634402765 ) ) ;
#18529 = DIRECTION ( 'NONE',  ( -1.000000000000000000, 0.000000000000000000, 0.000000000000000000 ) ) ;
#18530 = CARTESIAN_POINT ( 'NONE',  ( 4.999999999999999112, -8.475820894093002877, 4.057423117305363647 ) ) ;
#18531 = CARTESIAN_POINT ( 'NONE',  ( -66.05000000109247082, 7.933012699999995476, 14.99999999999999645 ) ) ;
#18532 = DIRECTION ( 'NONE',  ( -1.000000000000000000, 0.000000000000000000, 0.000000000000000000 ) ) ;
#18533 = VERTEX_POINT ( 'NONE', #23183 ) ;
#18534 = CARTESIAN_POINT ( 'NONE',  ( 4.154306624731035846, -2.398490048085128556, -3.721999068284417955 ) ) ;
#18535 = CARTESIAN_POINT ( 'NONE',  ( 4.000000000000001776, -1.656854249492379694, 12.43750000000001066 ) ) ;
#18536 = CARTESIAN_POINT ( 'NONE',  ( 72.50000000000000000, 9.999999999999998224, 14.99999999999999645 ) ) ;
#18537 = AXIS2_PLACEMENT_3D ( 'NONE', #20328, #20448, #13184 ) ;
#18538 = ORIENTED_EDGE ( 'NONE', *, *, #21526, .F. ) ;
#18539 = CARTESIAN_POINT ( 'NONE',  ( 28.99286915928345110, -8.974600000000002353, 5.000000000000079936 ) ) ;
#18540 = LINE ( 'NONE', #22006, #9863 ) ;
#18541 = DIRECTION ( 'NONE',  ( 0.000000000000000000, 1.000000000000000000, 3.491481338843133355E-15 ) ) ;
#18542 = VECTOR ( 'NONE', #17241, 1000.000000000000000 ) ;
#18543 = VECTOR ( 'NONE', #20590, 1000.000000000000000 ) ;
#18544 = CARTESIAN_POINT ( 'NONE',  ( -1.656854249492380138, -3.999999999999999112, 16.31250000273119838 ) ) ;
#18545 = ORIENTED_EDGE ( 'NONE', *, *, #19878, .F. ) ;
#18546 = LINE ( 'NONE', #345, #21358 ) ;
#18547 = EDGE_LOOP ( 'NONE', ( #12131, #16353, #2159 ) ) ;
#18548 = CARTESIAN_POINT ( 'NONE',  ( 0.000000000000000000, 8.461683424509315543, 2.223716399045600145 ) ) ;
#18549 = CARTESIAN_POINT ( 'NONE',  ( 9.920644283265380691E-16, 4.000000000000000000, 15.75000000000001066 ) ) ;
#18550 = DIRECTION ( 'NONE',  ( 1.000000000000000000, 0.000000000000000000, 0.000000000000000000 ) ) ;
#18551 = ADVANCED_FACE ( 'NONE', ( #14116 ), #16025, .T. ) ;
#18552 = DIRECTION ( 'NONE',  ( 1.000000000000000000, 0.000000000000000000, 0.000000000000000000 ) ) ;
#18553 = EDGE_CURVE ( 'NONE', #13175, #683, #3130, .T. ) ;
#18554 = CARTESIAN_POINT ( 'NONE',  ( 0.000000000000000000, 0.000000000000000000, 0.000000000000000000 ) ) ;
#18555 = CARTESIAN_POINT ( 'NONE',  ( 69.55000000109247082, 11.46158073645647235, 13.53841926354352232 ) ) ;
#18556 = VERTEX_POINT ( 'NONE', #1973 ) ;
#18557 = AXIS2_PLACEMENT_3D ( 'NONE', #5675, #11212, #13129 ) ;
#18558 = CARTESIAN_POINT ( 'NONE',  ( 5.434916218090830142, 4.367703157927330437, -0.2578475836320699988 ) ) ;
#18559 = CIRCLE ( 'NONE', #949, 8.749000000000002331 ) ;
#18560 = FACE_OUTER_BOUND ( 'NONE', #10179, .T. ) ;
#18561 = EDGE_CURVE ( 'NONE', #18607, #4290, #7514, .T. ) ;
#18562 = CARTESIAN_POINT ( 'NONE',  ( 66.80000000109247082, 9.143825827087050939, 12.93301269999999370 ) ) ;
#18563 = CARTESIAN_POINT ( 'NONE',  ( -3.458734124999998993, -1.432654583217642497, 15.50000000136560807 ) ) ;
#18564 = DIRECTION ( 'NONE',  ( 0.000000000000000000, 0.000000000000000000, 1.000000000000000000 ) ) ;
#18565 = CARTESIAN_POINT ( 'NONE',  ( 3.458734125000000770, 4.235727675282972223E-16, -0.5124999986344038749 ) ) ;
#18566 = CARTESIAN_POINT ( 'NONE',  ( 4.000000000000000888, -1.656854249492379694, 5.737500000000000711 ) ) ;
#18567 = CARTESIAN_POINT ( 'NONE',  ( 2.828427124746190735, -2.828427124746189847, -3.199999997268812901 ) ) ;
#18568 = CARTESIAN_POINT ( 'NONE',  ( -2.445694354108819191, 2.445694354108820523, 14.31250000136560452 ) ) ;
#18569 = CARTESIAN_POINT ( 'NONE',  ( 1.236993788156008760E-15, 0.000000000000000000, 21.31370849898476649 ) ) ;
#18570 = AXIS2_PLACEMENT_3D ( 'NONE', #2603, #4410, #13427 ) ;
#18571 = VECTOR ( 'NONE', #22837, 1000.000000000000000 ) ;
#18572 = VERTEX_POINT ( 'NONE', #7400 ) ;
#18573 = CARTESIAN_POINT ( 'NONE',  ( -68.40000000109249356, 9.143825827087052716, 12.93301269999999192 ) ) ;
#18574 = ORIENTED_EDGE ( 'NONE', *, *, #8231, .T. ) ;
#18575 = CARTESIAN_POINT ( 'NONE',  ( 59.71875000000000711, 14.00000000000000888, 16.65685424949235482 ) ) ;
#18576 = CARTESIAN_POINT ( 'NONE',  ( -71.55000000109245661, 8.538419263543522320, 16.46158073645647235 ) ) ;
#18577 = APPLICATION_PROTOCOL_DEFINITION ( 'draft international standard', 'automotive_design', 1998, #3804 ) ;
#18578 = EDGE_LOOP ( 'NONE', ( #19928, #13863, #2292, #3374 ) ) ;
#18579 = DIRECTION ( 'NONE',  ( 1.000000000000000000, 0.000000000000000000, 0.000000000000000000 ) ) ;
#18580 = ORIENTED_EDGE ( 'NONE', *, *, #452, .F. ) ;
#18581 = AXIS2_PLACEMENT_3D ( 'NONE', #16066, #13925, #6833 ) ;
#18582 = VERTEX_POINT ( 'NONE', #3895 ) ;
#18583 = VECTOR ( 'NONE', #9553, 1000.000000000000000 ) ;
#18584 = CARTESIAN_POINT ( 'NONE',  ( 1.432654583217641386, 3.458734125000000770, 17.37500000136560274 ) ) ;
#18585 = CARTESIAN_POINT ( 'NONE',  ( 54.46875000000000000, 6.999999999999992895, 13.75735931288071967 ) ) ;
#18586 = CARTESIAN_POINT ( 'NONE',  ( -68.80000000109247082, 10.85617417291294551, 17.06698729999999742 ) ) ;
#18587 = EDGE_CURVE ( 'NONE', #2784, #6494, #6058, .T. ) ;
#18588 = CARTESIAN_POINT ( 'NONE',  ( 69.40000000109249356, 12.06698729999999919, 14.14382582708705094 ) ) ;
#18589 = CARTESIAN_POINT ( 'NONE',  ( -71.30000000109247082, 12.06698730000000275, 15.85617417291294196 ) ) ;
#18590 =( BOUNDED_CURVE ( )  B_SPLINE_CURVE ( 2, ( #14127, #7049, #5012, #17600, #16156, #8860, #12221, #14366, #2958 ),
 .UNSPECIFIED., .F., .F. ) 
 B_SPLINE_CURVE_WITH_KNOTS ( ( 3, 2, 2, 2, 3 ),
 ( 0.8749999999999990008, 0.8906249999999994449, 0.9062499999999998890, 0.9218750000000003331, 0.9375000000000007772 ),
 .UNSPECIFIED. ) 
 CURVE ( )  GEOMETRIC_REPRESENTATION_ITEM ( )  RATIONAL_B_SPLINE_CURVE ( ( 1.000000000000004885, 0.9238795325112818535, 1.000000000000000000, 0.9238795325112867385, 1.000000000000000000, 0.9238795325112867385, 1.000000000000000000, 0.9238795325112829637, 1.000000000000003775 ) ) 
 REPRESENTATION_ITEM ( '' )  );
#18591 = CARTESIAN_POINT ( 'NONE',  ( 3.458734125000002546, -1.432654583217639610, 12.12500000136560629 ) ) ;
#18592 = CARTESIAN_POINT ( 'NONE',  ( 67.70000000000000284, 9.999999999999998224, 17.49999999999999645 ) ) ;
#18593 = EDGE_CURVE ( 'NONE', #19389, #13563, #67, .T. ) ;
#18594 = CARTESIAN_POINT ( 'NONE',  ( 59.49768183416157541, 12.16943976678977535, 12.92679907967048614 ) ) ;
#18595 = EDGE_CURVE ( 'NONE', #12636, #7229, #5700, .T. ) ;
#18596 = CARTESIAN_POINT ( 'NONE',  ( 55.31250000000000711, 13.00000000000000000, 14.99999999999998757 ) ) ;
#18597 = CARTESIAN_POINT ( 'NONE',  ( 3.458734125000001214, 4.235727675282971730E-16, 10.93750000136560452 ) ) ;
#18598 = CARTESIAN_POINT ( 'NONE',  ( 9.920644283265380691E-16, 4.000000000000000000, 14.87500000273119660 ) ) ;
#18599 = DIRECTION ( 'NONE',  ( -1.000000000000000000, -7.703719777548943412E-32, 0.000000000000000000 ) ) ;
#18600 = ORIENTED_EDGE ( 'NONE', *, *, #551, .T. ) ;
#18601 = CARTESIAN_POINT ( 'NONE',  ( 25.00005080000000035, 5.400000000000000355, 1.000000000000000000 ) ) ;
#18602 = CARTESIAN_POINT ( 'NONE',  ( -0.6810597143197697489, -4.461075778259609770, -3.598441714920717516 ) ) ;
#18603 = ORIENTED_EDGE ( 'NONE', *, *, #20957, .T. ) ;
#18604 = CARTESIAN_POINT ( 'NONE',  ( 60.52893183416158251, 11.17458954617365663, 18.02818770551464311 ) ) ;
#18605 = CARTESIAN_POINT ( 'NONE',  ( -2.445694354108819635, -2.445694354108820523, 3.862500001365594571 ) ) ;
#18606 = CARTESIAN_POINT ( 'NONE',  ( 1.763857611550045723, 3.892996637942334637, 1.981791682344426375 ) ) ;
#18607 = VERTEX_POINT ( 'NONE', #22207 ) ;
#18608 = CARTESIAN_POINT ( 'NONE',  ( -3.999999999999998224, -1.656854249492383246, 12.06250000000001243 ) ) ;
#18609 = DIRECTION ( 'NONE',  ( 1.000000000000000000, 7.703719777548943412E-32, 0.000000000000000000 ) ) ;
#18610 = CARTESIAN_POINT ( 'NONE',  ( -65.52500000163871618, 9.999999999999998224, 17.28349365000000049 ) ) ;
#18611 = EDGE_LOOP ( 'NONE', ( #14333, #15460, #8582, #6098 ) ) ;
#18612 = CARTESIAN_POINT ( 'NONE',  ( -20.00000000000001066, -10.00000000000000000, -49.99999999999999289 ) ) ;
#18613 = CYLINDRICAL_SURFACE ( 'NONE', #12553, 4.000000000000001776 ) ;
#18614 = EDGE_CURVE ( 'NONE', #22160, #21976, #13391, .T. ) ;
#18615 = CARTESIAN_POINT ( 'NONE',  ( 67.59999999999999432, 11.76776695296636888, 16.76776695296636532 ) ) ;
#18616 = EDGE_CURVE ( 'NONE', #2705, #7575, #2359, .T. ) ;
#18617 = DIRECTION ( 'NONE',  ( -1.000000000000000000, -7.703719777548943412E-32, 0.000000000000000000 ) ) ;
#18618 = AXIS2_PLACEMENT_3D ( 'NONE', #14940, #13602, #15174 ) ;
#18619 = EDGE_CURVE ( 'NONE', #2759, #7447, #5580, .T. ) ;
#18620 = FACE_OUTER_BOUND ( 'NONE', #18839, .T. ) ;
#18621 = CARTESIAN_POINT ( 'NONE',  ( 58.25231816583843170, 7.926799079670502124, 17.16943976678978245 ) ) ;
#18622 = CARTESIAN_POINT ( 'NONE',  ( -1.432654583217640498, 3.458734125000000770, 4.800000001365595459 ) ) ;
#18623 = CARTESIAN_POINT ( 'NONE',  ( 2.445694354108822299, -2.445694354108820079, 13.06250000136560629 ) ) ;
#18624 =( NAMED_UNIT ( * ) PLANE_ANGLE_UNIT ( ) SI_UNIT ( $, .RADIAN. ) );
#18625 = CARTESIAN_POINT ( 'NONE',  ( 65.52500000163871618, 9.999999999999998224, 17.28349365000000049 ) ) ;
#18626 =( BOUNDED_CURVE ( )  B_SPLINE_CURVE ( 2, ( #12244, #1295, #16057, #7070, #10804, #1540, #23213, #17731, #5383, #3109, #8881, #19974, #12722, #23584, #3577, #9116, #13389, #10684, #12478, #21413, #16174, #14147, #18077, #12360, #16404, #15935, #19742, #5140, #23462, #14269, #10450, #17960, #3342, #19512, #5029, #1658, #23347, #1774, #7321, #10912, #10569, #8750, #3219, #14387, #21649, #19622, #18192, #17841, #5259, #14626, #8632, #21886, #21531, #6954, #12602, #19863, #1410, #3466, #9000, #16293, #7194, #14509, #21773, #7782, #18425, #16521, #16755, #13294, #13067, #14991, #22241, #5496, #97, #16882, #7895, #20441, #12828, #5849, #568, #20206, #9589, #5971, #2002, #12942, #9457, #13178, #20087, #11027, #4051, #22357, #16996, #3686, #3815, #9237, #18310, #1893, #11380 ),
 .UNSPECIFIED., .F., .F. ) 
 B_SPLINE_CURVE_WITH_KNOTS ( ( 3, 2, 2, 2, 2, 2, 2, 2, 2, 2, 2, 2, 2, 2, 2, 2, 2, 2, 2, 2, 2, 2, 2, 2, 2, 2, 2, 2, 2, 2, 2, 2, 2, 2, 2, 2, 2, 2, 2, 2, 2, 2, 2, 2, 2, 2, 2, 2, 3 ),
 ( 0.000000000000000000, 0.02083333333333333218, 0.04166666666666666435, 0.06250000000000000000, 0.08333333333333332871, 0.1041666666666666713, 0.1250000000000000000, 0.1458333333333333426, 0.1666666666666666574, 0.1875000000000000000, 0.2083333333333333426, 0.2291666666666666574, 0.2500000000000000000, 0.2708333333333333148, 0.2916666666666666852, 0.3125000000000000000, 0.3333333333333333148, 0.3541666666666666852, 0.3750000000000000000, 0.3958333333333333148, 0.4166666666666666852, 0.4375000000000000000, 0.4583333333333333148, 0.4791666666666666852, 0.5000000000000000000, 0.5208333333333333703, 0.5416666666666666297, 0.5625000000000000000, 0.5833333333333333703, 0.6041666666666666297, 0.6250000000000000000, 0.6458333333333333703, 0.6666666666666666297, 0.6875000000000000000, 0.7083333333333333703, 0.7291666666666666297, 0.7500000000000000000, 0.7708333333333333703, 0.7916666666666666297, 0.8125000000000000000, 0.8333333333333333703, 0.8541666666666666297, 0.8750000000000000000, 0.8958333333333333703, 0.9166666666666666297, 0.9375000000000000000, 0.9583333333333333703, 0.9791666666666666297, 1.000000000000000000 ),
 .UNSPECIFIED. ) 
 CURVE ( )  GEOMETRIC_REPRESENTATION_ITEM ( )  RATIONAL_B_SPLINE_CURVE ( ( 1.000000000000000000, 0.9238795325112867385, 1.000000000000000000, 0.9238795325112867385, 1.000000000000000000, 0.9238795325112867385, 1.000000000000000000, 0.9238795325112867385, 1.000000000000000000, 0.9238795325112867385, 1.000000000000000000, 0.9238795325112867385, 1.000000000000000000, 0.9238795325112867385, 1.000000000000000000, 0.9238795325112867385, 1.000000000000000000, 0.9238795325112867385, 1.000000000000000000, 0.9238795325112867385, 1.000000000000000000, 0.9238795325112867385, 1.000000000000000000, 0.9238795325112867385, 1.000000000000000000, 0.9238795325112867385, 1.000000000000000000, 0.9238795325112867385, 1.000000000000000000, 0.9238795325112867385, 1.000000000000000000, 0.9238795325112867385, 1.000000000000000000, 0.9238795325112867385, 1.000000000000000000, 0.9238795325112867385, 1.000000000000000000, 0.9238795325112867385, 1.000000000000000000, 0.9238795325112867385, 1.000000000000000000, 0.9238795325112867385, 1.000000000000000000, 0.9238795325112867385, 1.000000000000000000, 0.9238795325112867385, 1.000000000000000000, 0.9238795325112867385, 1.000000000000000000, 0.9238795325112867385, 1.000000000000000000, 0.9238795325112867385, 1.000000000000000000, 0.9238795325112867385, 1.000000000000000000, 0.9238795325112867385, 1.000000000000000000, 0.9238795325112867385, 1.000000000000000000, 0.9238795325112867385, 1.000000000000000000, 0.9238795325112867385, 1.000000000000000000, 0.9238795325112867385, 1.000000000000000000, 0.9238795325112867385, 1.000000000000000000, 0.9238795325112867385, 1.000000000000000000, 0.9238795325112867385, 1.000000000000000000, 0.9238795325112867385, 1.000000000000000000, 0.9238795325112867385, 1.000000000000000000, 0.9238795325112867385, 1.000000000000000000, 0.9238795325112867385, 1.000000000000000000, 0.9238795325112867385, 1.000000000000000000, 0.9238795325112867385, 1.000000000000000000, 0.9238795325112867385, 1.000000000000000000, 0.9238795325112867385, 1.000000000000000000, 0.9238795325112867385, 1.000000000000000000, 0.9238795325112867385, 1.000000000000000000, 0.9238795325112867385, 1.000000000000000000, 0.9238795325112867385, 1.000000000000000000, 0.9238795325112867385, 1.000000000000000000 ) ) 
 REPRESENTATION_ITEM ( '' )  );
#18627 = AXIS2_PLACEMENT_3D ( 'NONE', #12739, #1313, #19989 ) ;
#18628 = DIRECTION ( 'NONE',  ( -1.000000000000000000, 0.000000000000000000, 0.000000000000000000 ) ) ;
#18629 = ORIENTED_EDGE ( 'NONE', *, *, #21797, .F. ) ;
#18630 = CARTESIAN_POINT ( 'NONE',  ( -20.00005079999999680, 0.000000000000000000, 0.000000000000000000 ) ) ;
#18631 = CARTESIAN_POINT ( 'NONE',  ( 0.000000000000000000, 0.000000000000000000, 0.000000000000000000 ) ) ;
#18632 = CARTESIAN_POINT ( 'NONE',  ( -71.45000000109247651, 7.933012699999995476, 14.99999999999999645 ) ) ;
#18633 = EDGE_LOOP ( 'NONE', ( #2720, #9741, #1639, #8453 ) ) ;
#18634 = VERTEX_POINT ( 'NONE', #298 ) ;
#18635 = VECTOR ( 'NONE', #1463, 1000.000000000000114 ) ;
#18636 =( NAMED_UNIT ( * ) PLANE_ANGLE_UNIT ( ) SI_UNIT ( $, .RADIAN. ) );
#18637 = CARTESIAN_POINT ( 'NONE',  ( 58.03125000000000711, 11.65685424949239923, 18.99999999999998934 ) ) ;
#18638 = ORIENTED_EDGE ( 'NONE', *, *, #1739, .F. ) ;
#18639 = LINE ( 'NONE', #6196, #20218 ) ;
#18640 = EDGE_LOOP ( 'NONE', ( #15733, #926, #11249, #20802 ) ) ;
#18641 = STYLED_ITEM ( 'NONE', ( #23168 ), #6561 ) ;
#18642 = PRODUCT_DEFINITION_CONTEXT ( 'detailed design', #1801, 'design' ) ;
#18643 = CARTESIAN_POINT ( 'NONE',  ( 57.31481816583843170, 14.00000000000000178, 14.93194885905434610 ) ) ;
#18644 = CARTESIAN_POINT ( 'NONE',  ( 72.05000000109247082, 9.999999999999998224, 17.06698730000000097 ) ) ;
#18645 = CARTESIAN_POINT ( 'NONE',  ( 1.656854249492381470, 4.000000000000000000, 19.68750000000001066 ) ) ;
#18646 = FACE_OUTER_BOUND ( 'NONE', #6960, .T. ) ;
#18647 = ORIENTED_EDGE ( 'NONE', *, *, #15707, .T. ) ;
#18648 = CARTESIAN_POINT ( 'NONE',  ( -2.828427124746189403, 2.828427124746190291, 14.00000000273119660 ) ) ;
#18649 = AXIS2_PLACEMENT_3D ( 'NONE', #9773, #17071, #6288 ) ;
#18650 = DIRECTION ( 'NONE',  ( -0.000000000000000000, -1.000000000000000000, -0.000000000000000000 ) ) ;
#18651 = CARTESIAN_POINT ( 'NONE',  ( 51.99768183416157541, 12.87654654797631792, 12.21969229848393113 ) ) ;
#18652 = CARTESIAN_POINT ( 'NONE',  ( 3.422634207080918589, -1.398009529842456855, 2.039999999999996927 ) ) ;
#18653 = DIRECTION ( 'NONE',  ( 0.000000000000000000, 0.000000000000000000, -1.000000000000000000 ) ) ;
#18654 = CARTESIAN_POINT ( 'NONE',  ( 0.000000000000000000, 1.464956435139695978, -10.90201369670497122 ) ) ;
#18655 = VECTOR ( 'NONE', #19932, 1000.000000000000000 ) ;
#18656 = AXIS2_PLACEMENT_3D ( 'NONE', #10402, #410, #20035 ) ;
#18657 = DIRECTION ( 'NONE',  ( -1.000000000000000000, 0.000000000000000000, 0.000000000000000000 ) ) ;
#18658 = CARTESIAN_POINT ( 'NONE',  ( 45.00000000000000000, 10.00000000000001599, 12.50000000000002842 ) ) ;
#18659 = ORIENTED_EDGE ( 'NONE', *, *, #8964, .F. ) ;
#18660 = CARTESIAN_POINT ( 'NONE',  ( -4.000000000000000000, -0.8382240730041925492, -3.220610619767135141 ) ) ;
#18661 = LINE ( 'NONE', #21887, #16211 ) ;
#18662 = EDGE_LOOP ( 'NONE', ( #10801, #5701, #12755, #17711 ) ) ;
#18663 = ADVANCED_FACE ( 'NONE', ( #11354, #15185 ), #7863, .T. ) ;
#18664 = DIRECTION ( 'NONE',  ( 0.3420201433256622181, 0.9396926207859107594, -6.162975822039141593E-32 ) ) ;
#18665 = VECTOR ( 'NONE', #5789, 1000.000000000000000 ) ;
#18666 = CARTESIAN_POINT ( 'NONE',  ( 4.000000000000000888, 4.898587196589412829E-16, 21.31370849898476649 ) ) ;
#18667 = DIRECTION ( 'NONE',  ( 0.000000000000000000, 0.000000000000000000, -1.000000000000000000 ) ) ;
#18668 = DIRECTION ( 'NONE',  ( 1.000000000000000000, 0.000000000000000000, 0.000000000000000000 ) ) ;
#18669 = VERTEX_POINT ( 'NONE', #18504 ) ;
#18670 = CARTESIAN_POINT ( 'NONE',  ( 0.2615509004163102946, 3.991439731035835603, 2.039999999999998259 ) ) ;
#18671 = ORIENTED_EDGE ( 'NONE', *, *, #18128, .F. ) ;
#18672 = CIRCLE ( 'NONE', #16766, 8.073750000000021743 ) ;
#18673 = CARTESIAN_POINT ( 'NONE',  ( -4.000000000000000000, -1.656854249492383024, 1.362500000000001377 ) ) ;
#18674 = CARTESIAN_POINT ( 'NONE',  ( 2.828427124746191179, 2.828427124746190291, 15.62500000000001066 ) ) ;
#18675 = DIRECTION ( 'NONE',  ( -1.000000000000000000, 0.000000000000000000, 0.000000000000000000 ) ) ;
#18676 = VECTOR ( 'NONE', #23652, 1000.000000000000000 ) ;
#18677 = VECTOR ( 'NONE', #11811, 1000.000000000000000 ) ;
#18678 = LINE ( 'NONE', #17010, #4961 ) ;
#18679 = STYLED_ITEM ( 'NONE', ( #3288 ), #20459 ) ;
#18680 = DIRECTION ( 'NONE',  ( -0.000000000000000000, -0.000000000000000000, 1.000000000000000000 ) ) ;
#18681 = CARTESIAN_POINT ( 'NONE',  ( 71.45000000109247651, 9.999999999999998224, 17.06698730000000097 ) ) ;
#18682 = ORIENTED_EDGE ( 'NONE', *, *, #2824, .F. ) ;
#18683 = DIRECTION ( 'NONE',  ( 1.000000000000000000, 0.000000000000000000, 0.000000000000000000 ) ) ;
#18684 = DIRECTION ( 'NONE',  ( 0.000000000000000000, 0.000000000000000000, -1.000000000000000000 ) ) ;
#18685 = CARTESIAN_POINT ( 'NONE',  ( 72.05000000109245661, 12.06698730000000097, 14.99999999999999645 ) ) ;
#18686 = CARTESIAN_POINT ( 'NONE',  ( 3.458734125000002102, -1.432654583217639610, 16.87500000136560629 ) ) ;
#18687 = CARTESIAN_POINT ( 'NONE',  ( 2.500000000000000000, -1.768423874527823569, 1.021000000000002350 ) ) ;
#18688 = AXIS2_PLACEMENT_3D ( 'NONE', #358, #18683, #7691 ) ;
#18689 = CARTESIAN_POINT ( 'NONE',  ( -1.432654583217641164, -3.458734125000000326, -1.824999998634404097 ) ) ;
#18690 = CARTESIAN_POINT ( 'NONE',  ( -1.656854249492381248, -3.999999999999999112, 2.487500000000002043 ) ) ;
#18691 = CARTESIAN_POINT ( 'NONE',  ( 3.458734125000001214, 4.235727675282971730E-16, 14.93750000136560452 ) ) ;
#18692 = CYLINDRICAL_SURFACE ( 'NONE', #2678, 4.000000000000001776 ) ;
#18693 = ORIENTED_EDGE ( 'NONE', *, *, #1844, .F. ) ;
#18694 = ADVANCED_FACE ( 'NONE', ( #13033 ), #20291, .T. ) ;
#18695 = CARTESIAN_POINT ( 'NONE',  ( -66.80000000109247082, 9.143825827087052716, 12.93301269999999192 ) ) ;
#18696 = ORIENTED_EDGE ( 'NONE', *, *, #20202, .F. ) ;
#18697 = CARTESIAN_POINT ( 'NONE',  ( 59.06250000000000711, 5.999999999999996447, 15.00000000000001599 ) ) ;
#18698 = CARTESIAN_POINT ( 'NONE',  ( -71.20000000109246230, 12.06698730000000275, 14.14382582708705094 ) ) ;
#18699 = APPLICATION_PROTOCOL_DEFINITION ( 'draft international standard', 'automotive_design', 1998, #5946 ) ;
#18700 = VECTOR ( 'NONE', #1389, 1000.000000000000000 ) ;
#18701 = ORIENTED_EDGE ( 'NONE', *, *, #2934, .F. ) ;
#18702 = DIRECTION ( 'NONE',  ( 0.000000000000000000, -0.000000000000000000, 1.000000000000000000 ) ) ;
#18703 = ORIENTED_EDGE ( 'NONE', *, *, #16977, .F. ) ;
#18704 = ORIENTED_EDGE ( 'NONE', *, *, #12761, .T. ) ;
#18705 = CARTESIAN_POINT ( 'NONE',  ( -2.445694354108818303, -2.445694354108820967, 17.81250000136560274 ) ) ;
#18706 = VECTOR ( 'NONE', #8743, 1000.000000000000000 ) ;
#18707 = ADVANCED_FACE ( 'NONE', ( #7634 ), #14957, .T. ) ;
#18708 = CARTESIAN_POINT ( 'NONE',  ( 57.28125000000000711, 8.757359312880703683, 11.99999999999999822 ) ) ;
#18709 = AXIS2_PLACEMENT_3D ( 'NONE', #13287, #18650, #14851 ) ;
#18710 = CARTESIAN_POINT ( 'NONE',  ( -66.75000000109247367, 8.538419263543524096, 13.53841926354352054 ) ) ;
#18711 = CARTESIAN_POINT ( 'NONE',  ( 68.10000000109248219, 9.143825827087049163, 17.06698730000000097 ) ) ;
#18712 = PRODUCT_DEFINITION_FORMATION_WITH_SPECIFIED_SOURCE ( 'ANY', '', #11846, .NOT_KNOWN. ) ;
#18713 = CARTESIAN_POINT ( 'NONE',  ( -66.70000000109246230, 9.143825827087049163, 17.06698729999999742 ) ) ;
#18714 = AXIS2_PLACEMENT_3D ( 'NONE', #21494, #21734, #5106 ) ;
#18715 = FACE_OUTER_BOUND ( 'NONE', #17830, .T. ) ;
#18716 = CARTESIAN_POINT ( 'NONE',  ( 56.49768183416158962, 12.16943976678977535, 12.92679907967048614 ) ) ;
#18717 = DIRECTION ( 'NONE',  ( 1.224646799147353207E-16, -0.000000000000000000, 1.000000000000000000 ) ) ;
#18718 = CARTESIAN_POINT ( 'NONE',  ( -3.458734125000000770, 1.432654583217640498, 3.925000001365594127 ) ) ;
#18719 = CARTESIAN_POINT ( 'NONE',  ( 1.025207404391860050E-15, 3.458734125000000326, 12.18750000136560629 ) ) ;
#18720 = CARTESIAN_POINT ( 'NONE',  ( 4.000000000000001776, -1.656854249492379694, 17.56250000273119838 ) ) ;
#18721 = CARTESIAN_POINT ( 'NONE',  ( 68.74999999999998579, 7.499999999999996447, 13.96446609406725514 ) ) ;
#18722 = AXIS2_PLACEMENT_3D ( 'NONE', #11590, #5812, #7626 ) ;
#18723 = ORIENTED_EDGE ( 'NONE', *, *, #871, .F. ) ;
#18724 = EDGE_CURVE ( 'NONE', #15279, #22866, #15560, .T. ) ;
#18725 = LINE ( 'NONE', #22182, #20811 ) ;
#18726 = ORIENTED_EDGE ( 'NONE', *, *, #13309, .F. ) ;
#18727 = CARTESIAN_POINT ( 'NONE',  ( 56.40393183416158251, 13.02818770551463778, 13.82541045382633982 ) ) ;
#18728 = SHAPE_REPRESENTATION_RELATIONSHIP ( 'NONE' , 'NONE' ,  #1939, #8790 ) ;
#18729 = CARTESIAN_POINT ( 'NONE',  ( -3.458734124999999882, -1.432654583217642497, 1.800000001365597235 ) ) ;
#18730 = EDGE_CURVE ( 'NONE', #14904, #18283, #2213, .T. ) ;
#18731 = CARTESIAN_POINT ( 'NONE',  ( -3.802871176606132053, -5.309964801958122926, -0.01372220897662011427 ) ) ;
#18732 = EDGE_LOOP ( 'NONE', ( #7108, #12011, #16301, #8835 ) ) ;
#18733 = CARTESIAN_POINT ( 'NONE',  ( -3.999999999999998224, -1.656854249492383246, 14.06250000000001066 ) ) ;
#18734 = CARTESIAN_POINT ( 'NONE',  ( 0.000000000000000000, -4.762163868918205978, -9.915734732513268312 ) ) ;
#18735 = VECTOR ( 'NONE', #14681, 1000.000000000000000 ) ;
#18736 = DIRECTION ( 'NONE',  ( 0.000000000000000000, -1.000000000000000000, 1.287488025362403787E-15 ) ) ;
#18737 = ORIENTED_EDGE ( 'NONE', *, *, #8357, .T. ) ;
#18738 = EDGE_CURVE ( 'NONE', #3314, #16036, #3754, .T. ) ;
#18739 = ADVANCED_FACE ( 'NONE', ( #2810, #7988 ), #1010, .T. ) ;
#18740 = DIRECTION ( 'NONE',  ( 0.000000000000000000, 0.000000000000000000, -1.000000000000000000 ) ) ;
#18741 =( BOUNDED_CURVE ( )  B_SPLINE_CURVE ( 2, ( #10705, #17984, #8897, #118, #22142, #7449, #18334, #3952, #13200 ),
 .UNSPECIFIED., .F., .F. ) 
 B_SPLINE_CURVE_WITH_KNOTS ( ( 3, 2, 2, 2, 3 ),
 ( 0.8124999999999993339, 0.8281249999999992228, 0.8437499999999991118, 0.8593749999999991118, 0.8749999999999990008 ),
 .UNSPECIFIED. ) 
 CURVE ( )  GEOMETRIC_REPRESENTATION_ITEM ( )  RATIONAL_B_SPLINE_CURVE ( ( 1.000000000000003331, 0.9238795325112835188, 1.000000000000000000, 0.9238795325112867385, 1.000000000000000000, 0.9238795325112867385, 1.000000000000000000, 0.9238795325112916235, 0.9999999999999951150 ) ) 
 REPRESENTATION_ITEM ( '' )  );
#18742 = CARTESIAN_POINT ( 'NONE',  ( -2.445694354108819635, -2.445694354108820967, -0.8874999986344025427 ) ) ;
#18743 = VECTOR ( 'NONE', #14041, 1000.000000000000000 ) ;
#18744 = AXIS2_PLACEMENT_3D ( 'NONE', #18449, #7568, #18098 ) ;
#18745 = CARTESIAN_POINT ( 'NONE',  ( 50.00000000000000000, -2.399706452296352932, 60.00000000000021316 ) ) ;
#18746 = CARTESIAN_POINT ( 'NONE',  ( 67.84999999999999432, 7.499999999999995559, 16.03553390593273420 ) ) ;
#18747 = DIRECTION ( 'NONE',  ( 0.000000000000000000, 0.000000000000000000, -1.000000000000000000 ) ) ;
#18748 = AXIS2_PLACEMENT_3D ( 'NONE', #13174, #9113, #20439 ) ;
#18749 = DIRECTION ( 'NONE',  ( -1.000000000000000000, 0.000000000000000000, 0.000000000000000000 ) ) ;
#18750 = CARTESIAN_POINT ( 'NONE',  ( 53.28356816583845301, 8.275094609561968184, 11.02818770551464667 ) ) ;
#18751 = CARTESIAN_POINT ( 'NONE',  ( -2.445694354108819635, -2.445694354108820967, 5.112500001365595459 ) ) ;
#18752 = CARTESIAN_POINT ( 'NONE',  ( 1.432654583217641386, 3.458734125000000770, 15.37500000136560807 ) ) ;
#18753 = CARTESIAN_POINT ( 'NONE',  ( 60.00000000000000711, 12.82842712474617741, 12.17157287525379239 ) ) ;
#18754 = CARTESIAN_POINT ( 'NONE',  ( -67.29999999999999716, 9.999999999999998224, 12.49999999999999289 ) ) ;
#18755 = DIRECTION ( 'NONE',  ( 0.000000000000000000, 0.000000000000000000, 1.000000000000000000 ) ) ;
#18756 = ORIENTED_EDGE ( 'NONE', *, *, #974, .F. ) ;
#18757 = CYLINDRICAL_SURFACE ( 'NONE', #4596, 2.500000000000002220 ) ;
#18758 = FACE_OUTER_BOUND ( 'NONE', #12111, .T. ) ;
#18759 = EDGE_CURVE ( 'NONE', #23355, #19246, #15411, .T. ) ;
#18760 = CARTESIAN_POINT ( 'NONE',  ( -71.70000000109247651, 10.85617417291294551, 12.93301269999999370 ) ) ;
#18761 = ORIENTED_EDGE ( 'NONE', *, *, #15710, .T. ) ;
#18762 = EDGE_LOOP ( 'NONE', ( #19896, #2246, #13889, #16232 ) ) ;
#18763 = CARTESIAN_POINT ( 'NONE',  ( 0.000000000000000000, 0.000000000000000000, -3.700000000000000178 ) ) ;
#18764 = CARTESIAN_POINT ( 'NONE',  ( 4.999999999999999112, 4.729683950898977862, -7.360373001730867060 ) ) ;
#18765 = VERTEX_POINT ( 'NONE', #10151 ) ;
#18766 = CARTESIAN_POINT ( 'NONE',  ( 0.1221691407165617638, -8.974600000000002353, 5.000000000000079936 ) ) ;
#18767 = ORIENTED_EDGE ( 'NONE', *, *, #15505, .F. ) ;
#18768 = AXIS2_PLACEMENT_3D ( 'NONE', #22491, #14876, #5751 ) ;
#18769 = ADVANCED_FACE ( 'NONE', ( #18865 ), #2564, .T. ) ;
#18770 = CARTESIAN_POINT ( 'NONE',  ( 53.93981816583844591, 10.06805114094564857, 19.00000000000000000 ) ) ;
#18771 = AXIS2_PLACEMENT_3D ( 'NONE', #19042, #18928, #4787 ) ;
#18772 = CARTESIAN_POINT ( 'NONE',  ( 70.05000000109247082, 9.999999999999998224, 12.93301269999999192 ) ) ;
#18773 = CARTESIAN_POINT ( 'NONE',  ( -3.999999999999999112, 0.000000000000000000, 17.12500000273119838 ) ) ;
#18774 = CARTESIAN_POINT ( 'NONE',  ( 70.05000000109247082, 7.933012699999995476, 14.99999999999999645 ) ) ;
#18775 = EDGE_LOOP ( 'NONE', ( #15582, #16984 ) ) ;
#18776 = CARTESIAN_POINT ( 'NONE',  ( 2.828427124746192067, -2.828427124746189847, 12.50000000273119838 ) ) ;
#18777 =( BOUNDED_SURFACE ( )  B_SPLINE_SURFACE ( 1, 2, ( 
 ( #16428, #7343, #5405, #14767, #121, #11, #14650, #5878, #10935, #1795, #11050, #15011, #20468, #13202, #12742, #7695, #22020, #5636, #3709, #9481, #18336, #9142, #20347, #12969, #9022, #21799, #12849, #3841, #7567, #20231, #19993, #14533, #2146, #23605, #11176, #16780, #361, #3954, #22266, #4074, #11409, #18686, #11288, #16315, #7219, #3595, #7451, #9259, #18214, #18448, #2028, #16545, #20106, #21907, #14887, #5515, #1918, #9368, #16659, #234, #5763, #22144, #13091, #18563, #7806, #4313, #4550, #5994, #17372, #4431, #4196, #22506, #17018, #2506, #8048, #11538, #6357, #6116, #15363, #2744, #15122, #940, #11651, #13446, #11766, #20708, #10084, #482, #8163, #2391, #13554, #19035, #9723, #8279, #9840, #18808, #20821, #13321, #22384, #22744, #6476, #594, #21054, #15594, #22862, #4666, #18917, #13671, #17136, #2624, #9615, #13797, #12000, #15239, #7919, #6233, #9968, #2275, #20589, #17262, #19157, #16905, #712, #22630, #830, #15474, #20934, #11886, #21166, #15930, #10445, #17725, #10325, #2973, #17615, #15715, #1288, #8626, #1181, #8518, #16488, #4778, #12115, #21278, #1534, #7396, #64, #22987, #17954 ),
 ( #6704, #13908, #21965, #19377, #23207, #16051, #14141, #14708, #15821, #6819, #23093, #21406, #19505, #10204, #21524, #14018, #5024, #4902, #12238, #1060, #12354, #19616, #23340, #3103, #8745, #3214, #10561, #17836, #5135, #6949, #1404, #14264, #12472, #19735, #3336, #8398, #10679, #8876, #5577, #19266, #2854, #17492, #6592, #5815, #2210, #20655, #20406, #22321, #5937, #12905, #7511, #536, #15304, #4134, #20165, #13263, #7984, #3891, #16959, #20526, #20290, #11476, #13386, #15182, #11594, #1970, #4259, #9310, #11227, #18752, #22441, #14952, #9549, #180, #2336, #7859, #22578, #423, #5695, #9669, #3772, #11112, #17077, #651, #14824, #22077, #13030, #13142, #2447, #18501, #16846, #6054, #9782, #11351, #18862, #18390, #7750, #9427, #16600, #2087, #16716, #294, #7630, #22204, #4014, #15066, #18623, #1006, #10391, #8113, #11951, #19101, #20997, #6418, #20767, #8467, #2693, #22686, #6182, #780, #8572, #4370, #6541, #3042, #15879, #17672, #15422, #12061, #6298, #1233, #9907, #13733, #22804, #2806, #8222, #11709, #19216, #4617, #13502, #13615, #4729, #23043, #18976, #20877, #8338, #17202, #2559, #2916, #4486 ) ),
 .UNSPECIFIED., .F., .F., .F. ) 
 B_SPLINE_SURFACE_WITH_KNOTS ( ( 2, 2 ),
 ( 3, 2, 2, 2, 2, 2, 2, 2, 2, 2, 2, 2, 2, 2, 2, 2, 2, 2, 2, 2, 2, 2, 2, 2, 2, 2, 2, 2, 2, 2, 2, 2, 2, 2, 2, 2, 2, 2, 2, 2, 2, 2, 2, 2, 2, 2, 2, 2, 2, 2, 2, 2, 2, 2, 2, 2, 2, 2, 2, 2, 2, 2, 2, 2, 2, 2, 2, 2, 2, 2, 2, 2, 2, 2, 3 ),
 ( 0.000000000000000000, 1.000000000000000000 ),
 ( 0.000000000000000000, 0.01250000000000000069, 0.02500000000000000139, 0.03749999999999999861, 0.05000000000000000278, 0.06250000000000000000, 0.07499999999999999722, 0.08749999999999999445, 0.1000000000000000056, 0.1125000000000000028, 0.1250000000000000000, 0.1375000000000000111, 0.1499999999999999944, 0.1625000000000000056, 0.1749999999999999889, 0.1875000000000000000, 0.2000000000000000111, 0.2124999999999999944, 0.2250000000000000056, 0.2374999999999999889, 0.2500000000000000000, 0.2625000000000000111, 0.2750000000000000222, 0.2874999999999999778, 0.2999999999999999889, 0.3125000000000000000, 0.3250000000000000111, 0.3375000000000000222, 0.3499999999999999778, 0.3624999999999999889, 0.3750000000000000000, 0.3875000000000000111, 0.4000000000000000222, 0.4124999999999999778, 0.4249999999999999889, 0.4375000000000000000, 0.4500000000000000111, 0.4625000000000000222, 0.4749999999999999778, 0.4874999999999999889, 0.5000000000000000000, 0.5124999999999999556, 0.5250000000000000222, 0.5374999999999999778, 0.5500000000000000444, 0.5625000000000000000, 0.5749999999999999556, 0.5875000000000000222, 0.5999999999999999778, 0.6125000000000000444, 0.6250000000000000000, 0.6374999999999999556, 0.6500000000000000222, 0.6624999999999999778, 0.6750000000000000444, 0.6875000000000000000, 0.6999999999999999556, 0.7125000000000000222, 0.7249999999999999778, 0.7375000000000000444, 0.7500000000000000000, 0.7624999999999999556, 0.7750000000000000222, 0.7874999999999999778, 0.8000000000000000444, 0.8125000000000000000, 0.8249999999999999556, 0.8375000000000000222, 0.8499999999999999778, 0.8625000000000000444, 0.8750000000000000000, 0.8874999999999999556, 0.9000000000000000222, 0.9124999999999999778, 0.9250000000000000444 ),
 .UNSPECIFIED. ) 
 GEOMETRIC_REPRESENTATION_ITEM ( )  RATIONAL_B_SPLINE_SURFACE ( (
 ( 1.000000000000000000, 0.9238795325112867385, 1.000000000000000000, 0.9238795325112867385, 1.000000000000000000, 0.9238795325112867385, 1.000000000000000000, 0.9238795325112867385, 1.000000000000000000, 0.9238795325112867385, 1.000000000000000000, 0.9238795325112867385, 1.000000000000000000, 0.9238795325112867385, 1.000000000000000000, 0.9238795325112867385, 1.000000000000000000, 0.9238795325112867385, 1.000000000000000000, 0.9238795325112867385, 1.000000000000000000, 0.9238795325112867385, 1.000000000000000000, 0.9238795325112867385, 1.000000000000000000, 0.9238795325112867385, 1.000000000000000000, 0.9238795325112867385, 1.000000000000000000, 0.9238795325112867385, 1.000000000000000000, 0.9238795325112867385, 1.000000000000000000, 0.9238795325112867385, 1.000000000000000000, 0.9238795325112867385, 1.000000000000000000, 0.9238795325112867385, 1.000000000000000000, 0.9238795325112867385, 1.000000000000000000, 0.9238795325112867385, 1.000000000000000000, 0.9238795325112867385, 1.000000000000000000, 0.9238795325112867385, 1.000000000000000000, 0.9238795325112867385, 1.000000000000000000, 0.9238795325112867385, 1.000000000000000000, 0.9238795325112867385, 1.000000000000000000, 0.9238795325112867385, 1.000000000000000000, 0.9238795325112867385, 1.000000000000000000, 0.9238795325112867385, 1.000000000000000000, 0.9238795325112867385, 1.000000000000000000, 0.9238795325112867385, 1.000000000000000000, 0.9238795325112867385, 1.000000000000000000, 0.9238795325112867385, 1.000000000000000000, 0.9238795325112867385, 1.000000000000000000, 0.9238795325112867385, 1.000000000000000000, 0.9238795325112867385, 1.000000000000000000, 0.9238795325112867385, 1.000000000000000000, 0.9238795325112867385, 1.000000000000000000, 0.9238795325112867385, 1.000000000000000000, 0.9238795325112867385, 1.000000000000000000, 0.9238795325112867385, 1.000000000000000000, 0.9238795325112867385, 1.000000000000000000, 0.9238795325112867385, 1.000000000000000000, 0.9238795325112867385, 1.000000000000000000, 0.9238795325112867385, 1.000000000000000000, 0.9238795325112867385, 1.000000000000000000, 0.9238795325112867385, 1.000000000000000000, 0.9238795325112867385, 1.000000000000000000, 0.9238795325112867385, 1.000000000000000000, 0.9238795325112867385, 1.000000000000000000, 0.9238795325112867385, 1.000000000000000000, 0.9238795325112867385, 1.000000000000000000, 0.9238795325112867385, 1.000000000000000000, 0.9238795325112867385, 1.000000000000000000, 0.9238795325112867385, 1.000000000000000000, 0.9238795325112867385, 1.000000000000000000, 0.9238795325112867385, 1.000000000000000000, 0.9238795325112867385, 1.000000000000000000, 0.9238795325112867385, 1.000000000000000000, 0.9238795325112867385, 1.000000000000000000, 0.9238795325112867385, 1.000000000000000000, 0.9238795325112867385, 1.000000000000000000, 0.9238795325112867385, 1.000000000000000000, 0.9238795325112867385, 1.000000000000000000, 0.9238795325112867385, 1.000000000000000000, 0.9238795325112867385, 1.000000000000000000, 0.9238795325112867385, 1.000000000000000000, 0.9238795325112867385, 1.000000000000000000, 0.9238795325112867385, 1.000000000000000000, 0.9238795325112867385, 1.000000000000000000, 0.9238795325112867385, 1.000000000000000000, 0.9238795325112867385, 1.000000000000000000, 0.9238795325112867385, 1.000000000000000000, 0.9238795325112867385, 1.000000000000000000),
 ( 1.000000000000000000, 0.9238795325112867385, 1.000000000000000000, 0.9238795325112867385, 1.000000000000000000, 0.9238795325112867385, 1.000000000000000000, 0.9238795325112867385, 1.000000000000000000, 0.9238795325112867385, 1.000000000000000000, 0.9238795325112867385, 1.000000000000000000, 0.9238795325112867385, 1.000000000000000000, 0.9238795325112867385, 1.000000000000000000, 0.9238795325112867385, 1.000000000000000000, 0.9238795325112867385, 1.000000000000000000, 0.9238795325112867385, 1.000000000000000000, 0.9238795325112867385, 1.000000000000000000, 0.9238795325112867385, 1.000000000000000000, 0.9238795325112867385, 1.000000000000000000, 0.9238795325112867385, 1.000000000000000000, 0.9238795325112867385, 1.000000000000000000, 0.9238795325112867385, 1.000000000000000000, 0.9238795325112867385, 1.000000000000000000, 0.9238795325112867385, 1.000000000000000000, 0.9238795325112867385, 1.000000000000000000, 0.9238795325112867385, 1.000000000000000000, 0.9238795325112867385, 1.000000000000000000, 0.9238795325112867385, 1.000000000000000000, 0.9238795325112867385, 1.000000000000000000, 0.9238795325112867385, 1.000000000000000000, 0.9238795325112867385, 1.000000000000000000, 0.9238795325112867385, 1.000000000000000000, 0.9238795325112867385, 1.000000000000000000, 0.9238795325112867385, 1.000000000000000000, 0.9238795325112867385, 1.000000000000000000, 0.9238795325112867385, 1.000000000000000000, 0.9238795325112867385, 1.000000000000000000, 0.9238795325112867385, 1.000000000000000000, 0.9238795325112867385, 1.000000000000000000, 0.9238795325112867385, 1.000000000000000000, 0.9238795325112867385, 1.000000000000000000, 0.9238795325112867385, 1.000000000000000000, 0.9238795325112867385, 1.000000000000000000, 0.9238795325112867385, 1.000000000000000000, 0.9238795325112867385, 1.000000000000000000, 0.9238795325112867385, 1.000000000000000000, 0.9238795325112867385, 1.000000000000000000, 0.9238795325112867385, 1.000000000000000000, 0.9238795325112867385, 1.000000000000000000, 0.9238795325112867385, 1.000000000000000000, 0.9238795325112867385, 1.000000000000000000, 0.9238795325112867385, 1.000000000000000000, 0.9238795325112867385, 1.000000000000000000, 0.9238795325112867385, 1.000000000000000000, 0.9238795325112867385, 1.000000000000000000, 0.9238795325112867385, 1.000000000000000000, 0.9238795325112867385, 1.000000000000000000, 0.9238795325112867385, 1.000000000000000000, 0.9238795325112867385, 1.000000000000000000, 0.9238795325112867385, 1.000000000000000000, 0.9238795325112867385, 1.000000000000000000, 0.9238795325112867385, 1.000000000000000000, 0.9238795325112867385, 1.000000000000000000, 0.9238795325112867385, 1.000000000000000000, 0.9238795325112867385, 1.000000000000000000, 0.9238795325112867385, 1.000000000000000000, 0.9238795325112867385, 1.000000000000000000, 0.9238795325112867385, 1.000000000000000000, 0.9238795325112867385, 1.000000000000000000, 0.9238795325112867385, 1.000000000000000000, 0.9238795325112867385, 1.000000000000000000, 0.9238795325112867385, 1.000000000000000000, 0.9238795325112867385, 1.000000000000000000, 0.9238795325112867385, 1.000000000000000000, 0.9238795325112867385, 1.000000000000000000, 0.9238795325112867385, 1.000000000000000000, 0.9238795325112867385, 1.000000000000000000, 0.9238795325112867385, 1.000000000000000000, 0.9238795325112867385, 1.000000000000000000) ) ) 
 REPRESENTATION_ITEM ( '' )  SURFACE ( )  );
#18778 = CARTESIAN_POINT ( 'NONE',  ( 21.00000000000000355, 0.000000000000000000, 2.055000000000000160 ) ) ;
#18779 = CARTESIAN_POINT ( 'NONE',  ( 55.18518183416157541, 10.06805114094561659, 10.99999999999999645 ) ) ;
#18780 = CARTESIAN_POINT ( 'NONE',  ( -2.696295709017760611, -5.948846446048907666, -3.700000000000000622 ) ) ;
#18781 = CARTESIAN_POINT ( 'NONE',  ( 2.445694354108821411, 2.445694354108820523, 17.06250000136560629 ) ) ;
#18782 = AXIS2_PLACEMENT_3D ( 'NONE', #1885, #3916, #9229 ) ;
#18783 = DIRECTION ( 'NONE',  ( 0.000000000000000000, -0.7071067811865406894, 0.7071067811865545671 ) ) ;
#18784 = CARTESIAN_POINT ( 'NONE',  ( -66.00000000109245946, 7.933012699999995476, 15.85617417291294196 ) ) ;
#18785 = DIRECTION ( 'NONE',  ( 0.000000000000000000, 0.000000000000000000, 1.000000000000000000 ) ) ;
#18786 = ORIENTED_EDGE ( 'NONE', *, *, #7628, .F. ) ;
#18787 = CARTESIAN_POINT ( 'NONE',  ( 1.971781867644420635E-15, -4.000000000000000000, 12.25000000000001066 ) ) ;
#18788 = DIRECTION ( 'NONE',  ( -1.000000000000000000, 0.000000000000000000, 0.000000000000000000 ) ) ;
#18789 = ORIENTED_EDGE ( 'NONE', *, *, #5765, .F. ) ;
#18790 = CYLINDRICAL_SURFACE ( 'NONE', #5555, 8.749000000000002331 ) ;
#18791 = CARTESIAN_POINT ( 'NONE',  ( -2.499999999999999556, 3.061616997868382648E-16, 3.469446951953614189E-15 ) ) ;
#18792 = LINE ( 'NONE', #922, #20476 ) ;
#18793 = EDGE_CURVE ( 'NONE', #7048, #5335, #8472, .T. ) ;
#18794 = DIRECTION ( 'NONE',  ( 0.000000000000000000, 0.000000000000000000, 1.000000000000000000 ) ) ;
#18795 = ORIENTED_EDGE ( 'NONE', *, *, #23292, .F. ) ;
#18796 = CARTESIAN_POINT ( 'NONE',  ( 10.97149113033275114, -11.25000000000000355, 10.00000000000008882 ) ) ;
#18797 = ORIENTED_EDGE ( 'NONE', *, *, #21776, .F. ) ;
#18798 = CARTESIAN_POINT ( 'NONE',  ( 7.347880794884118750E-16, -4.000000000000000000, 1.550000000000000933 ) ) ;
#18799 = CARTESIAN_POINT ( 'NONE',  ( -3.999999999999998224, -1.656854249492383246, 14.06250000000001066 ) ) ;
#18800 = PLANE ( 'NONE',  #12296 ) ;
#18801 = DIRECTION ( 'NONE',  ( -1.000000000000000000, 0.000000000000000000, 0.000000000000000000 ) ) ;
#18802 = CARTESIAN_POINT ( 'NONE',  ( 4.000000000000000888, 1.656854249492381248, 17.68750000273119483 ) ) ;
#18803 = CARTESIAN_POINT ( 'NONE',  ( 70.60000000109246798, 10.85617417291294551, 17.06698730000000097 ) ) ;
#18804 = EDGE_LOOP ( 'NONE', ( #11328, #10278, #6980, #15157 ) ) ;
#18805 = DIRECTION ( 'NONE',  ( -1.000000000000000000, 0.000000000000000000, 0.000000000000000000 ) ) ;
#18806 = CARTESIAN_POINT ( 'NONE',  ( 20.55500000000001748, 3.061616997868384127E-16, -2.500000000000000888 ) ) ;
#18807 = CARTESIAN_POINT ( 'NONE',  ( 67.30000000109247082, 9.143825827087049163, 17.06698729999999742 ) ) ;
#18808 = CARTESIAN_POINT ( 'NONE',  ( -3.458734124999998993, -1.432654583217642497, 13.50000000136560452 ) ) ;
#18809 = LINE ( 'NONE', #5995, #18543 ) ;
#18810 = CARTESIAN_POINT ( 'NONE',  ( 3.458734125000000770, 4.235727675282972223E-16, -2.512499998634404097 ) ) ;
#18811 = CARTESIAN_POINT ( 'NONE',  ( 4.000000000000000000, 4.898587196589412829E-16, -0.1999999999999987899 ) ) ;
#18812 = CARTESIAN_POINT ( 'NONE',  ( 72.50000000000000000, 9.999999999999998224, 17.49999999999999645 ) ) ;
#18813 = CARTESIAN_POINT ( 'NONE',  ( 1.432654583217641164, 3.458734125000000326, 11.12500000136560452 ) ) ;
#18814 = LINE ( 'NONE', #3714, #6912 ) ;
#18815 = ORIENTED_EDGE ( 'NONE', *, *, #16227, .T. ) ;
#18816 = CARTESIAN_POINT ( 'NONE',  ( -66.45000000109247651, 9.999999999999998224, 17.06698730000000097 ) ) ;
#18817 = ORIENTED_EDGE ( 'NONE', *, *, #11564, .T. ) ;
#18818 = CARTESIAN_POINT ( 'NONE',  ( 57.65625000000002132, 6.000000000000004441, 16.65685424949239390 ) ) ;
#18819 = CARTESIAN_POINT ( 'NONE',  ( -70.30000000109248504, 10.85617417291294551, 12.93301269999999370 ) ) ;
#18820 = CONTEXT_DEPENDENT_SHAPE_REPRESENTATION ( #6721, #4358 ) ;
#18821 = EDGE_LOOP ( 'NONE', ( #5945, #4090, #19976, #13675 ) ) ;
#18822 = DIRECTION ( 'NONE',  ( 0.000000000000000000, 0.000000000000000000, 1.000000000000000000 ) ) ;
#18823 = ORIENTED_EDGE ( 'NONE', *, *, #6464, .F. ) ;
#18824 = ORIENTED_EDGE ( 'NONE', *, *, #5302, .T. ) ;
#18825 = CARTESIAN_POINT ( 'NONE',  ( -3.458734124999999437, 0.000000000000000000, 15.68750000136560629 ) ) ;
#18826 = CARTESIAN_POINT ( 'NONE',  ( 55.59375000000000711, 11.24264068711927322, 11.99999999999998934 ) ) ;
#18827 = CARTESIAN_POINT ( 'NONE',  ( -68.90000000109247935, 9.143825827087049163, 17.06698729999999742 ) ) ;
#18828 = CARTESIAN_POINT ( 'NONE',  ( 70.50000000109247367, 9.143825827087049163, 17.06698730000000097 ) ) ;
#18829 = EDGE_CURVE ( 'NONE', #17633, #19580, #20424, .T. ) ;
#18830 = CARTESIAN_POINT ( 'NONE',  ( -66.35000000109246798, 11.46158073645647235, 13.53841926354352232 ) ) ;
#18831 = CARTESIAN_POINT ( 'NONE',  ( 118.3095189484530181, 15.00000000000001954, 10.00000000000008882 ) ) ;
#18832 = CARTESIAN_POINT ( 'NONE',  ( 56.12268183416157541, 12.07320092032950676, 17.16943976678977180 ) ) ;
#18833 = CARTESIAN_POINT ( 'NONE',  ( -65.97500000054623115, 9.999999999999998224, 17.28349365000000049 ) ) ;
#18834 = CARTESIAN_POINT ( 'NONE',  ( 1.432654583217642275, -3.458734124999999882, 2.300000001365597679 ) ) ;
#18835 = CARTESIAN_POINT ( 'NONE',  ( 3.458734125000001214, 4.235727675282971730E-16, 11.93750000136560629 ) ) ;
#18836 = CARTESIAN_POINT ( 'NONE',  ( -2.828427124746188515, -2.828427124746190735, 17.25000000273119838 ) ) ;
#18837 = EDGE_CURVE ( 'NONE', #20113, #23104, #16162, .T. ) ;
#18838 = LINE ( 'NONE', #13121, #16842 ) ;
#18839 = EDGE_LOOP ( 'NONE', ( #10440, #20, #18600, #16007 ) ) ;
#18840 = CARTESIAN_POINT ( 'NONE',  ( 24.42673246966726452, -11.25000000000000355, 10.00000000000008882 ) ) ;
#18841 = ORIENTED_EDGE ( 'NONE', *, *, #19807, .T. ) ;
#18842 = CARTESIAN_POINT ( 'NONE',  ( 58.56018183416157541, 7.000000000000000000, 14.93194885905437097 ) ) ;
#18843 = CARTESIAN_POINT ( 'NONE',  ( 3.458734125000000770, -1.432654583217639610, 3.175000001365598568 ) ) ;
#18844 = CARTESIAN_POINT ( 'NONE',  ( -3.458734124999999882, -1.432654583217642275, 0.8000000013655964581 ) ) ;
#18845 = VERTEX_POINT ( 'NONE', #11598 ) ;
#18846 = CARTESIAN_POINT ( 'NONE',  ( 4.000000000000000888, 1.656854249492381248, 13.56250000000001066 ) ) ;
#18847 = CARTESIAN_POINT ( 'NONE',  ( 50.00000000000000711, -15.00000000000001954, 5.000000000000079936 ) ) ;
#18848 = CARTESIAN_POINT ( 'NONE',  ( -3.999999999999999112, 1.656854249492380582, 14.93750000000001066 ) ) ;
#18849 = EDGE_LOOP ( 'NONE', ( #19694, #19030, #19276, #18084, #17298, #16901 ) ) ;
#18850 = CARTESIAN_POINT ( 'NONE',  ( -71.00000000218494733, 9.999999999999998224, 17.49999999999999645 ) ) ;
#18851 = DIRECTION ( 'NONE',  ( -1.000000000000000000, 0.000000000000000000, 0.000000000000000000 ) ) ;
#18852 = EDGE_CURVE ( 'NONE', #18509, #20280, #17081, .T. ) ;
#18853 = LINE ( 'NONE', #9662, #18314 ) ;
#18854 = CARTESIAN_POINT ( 'NONE',  ( 66.74999999999998579, 12.50000000000000000, 16.03553390593273420 ) ) ;
#18855 = EDGE_CURVE ( 'NONE', #6890, #14629, #14749, .T. ) ;
#18856 = DIRECTION ( 'NONE',  ( -1.000000000000000000, -7.703719777548943412E-32, 0.000000000000000000 ) ) ;
#18857 = CARTESIAN_POINT ( 'NONE',  ( 68.15000000109247935, 8.538419263543522320, 16.46158073645647235 ) ) ;
#18858 = DIRECTION ( 'NONE',  ( 1.000000000000000000, 7.703719777548943412E-32, 0.000000000000000000 ) ) ;
#18859 = CARTESIAN_POINT ( 'NONE',  ( 58.15856816583844591, 7.028187705514647554, 16.31069182806492179 ) ) ;
#18860 = CONICAL_SURFACE ( 'NONE', #22285, 6.500000000000000888, 1.047197551196596521 ) ;
#18861 = CARTESIAN_POINT ( 'NONE',  ( -3.458734125000000770, 0.000000000000000000, 5.987500001365596347 ) ) ;
#18862 = CARTESIAN_POINT ( 'NONE',  ( -2.445694354108818303, -2.445694354108820967, 13.81250000136560629 ) ) ;
#18863 = EDGE_CURVE ( 'NONE', #1035, #21012, #18979, .T. ) ;
#18864 = CARTESIAN_POINT ( 'NONE',  ( -71.60000000109246798, 7.933012699999995476, 15.85617417291294196 ) ) ;
#18865 = FACE_OUTER_BOUND ( 'NONE', #9742, .T. ) ;
#18866 = ORIENTED_EDGE ( 'NONE', *, *, #8771, .F. ) ;
#18867 = CARTESIAN_POINT ( 'NONE',  ( 4.999999999999999112, -4.729683950898921907, 7.360373001730902587 ) ) ;
#18868 = CARTESIAN_POINT ( 'NONE',  ( -2.828427124746190291, 2.828427124746190291, 4.300000002731186655 ) ) ;
#18869 = CARTESIAN_POINT ( 'NONE',  ( -71.85000000109246798, 12.06698730000000097, 14.99999999999999645 ) ) ;
#18870 = ORIENTED_EDGE ( 'NONE', *, *, #3793, .F. ) ;
#18871 = ORIENTED_EDGE ( 'NONE', *, *, #7795, .T. ) ;
#18872 = DIRECTION ( 'NONE',  ( -1.000000000000000000, 0.000000000000000000, 0.000000000000000000 ) ) ;
#18873 =( BOUNDED_CURVE ( )  B_SPLINE_CURVE ( 2, ( #13073, #3934, #11269, #343, #16762, #18544, #2130, #9465, #15107 ),
 .UNSPECIFIED., .F., .F. ) 
 B_SPLINE_CURVE_WITH_KNOTS ( ( 3, 2, 2, 2, 3 ),
 ( 0.2500000000000000000, 0.2625000000000000111, 0.2750000000000000222, 0.2874999999999999778, 0.2999999999999999889 ),
 .UNSPECIFIED. ) 
 CURVE ( )  GEOMETRIC_REPRESENTATION_ITEM ( )  RATIONAL_B_SPLINE_CURVE ( ( 1.000000000000000000, 0.9238795325112867385, 1.000000000000000000, 0.9238795325112867385, 1.000000000000000000, 0.9238795325112867385, 1.000000000000000000, 0.9238795325112867385, 1.000000000000000000 ) ) 
 REPRESENTATION_ITEM ( '' )  );
#18874 = CARTESIAN_POINT ( 'NONE',  ( -20.00000000000000355, 4.500000000000003553, 2.449293598294706907E-15 ) ) ;
#18875 = ORIENTED_EDGE ( 'NONE', *, *, #2134, .F. ) ;
#18876 = CARTESIAN_POINT ( 'NONE',  ( 1.360585162435110629, -4.061296242128317857, -3.505054077164905024 ) ) ;
#18877 = AXIS2_PLACEMENT_3D ( 'NONE', #18150, #9305, #5811 ) ;
#18878 = UNCERTAINTY_MEASURE_WITH_UNIT (LENGTH_MEASURE( 1.000000000000000082E-05 ), #10914, 'distance_accuracy_value', 'NONE');
#18879 = EDGE_CURVE ( 'NONE', #3586, #9317, #786, .T. ) ;
#18880 = CARTESIAN_POINT ( 'NONE',  ( 69.05000000109247082, 7.933012699999995476, 14.99999999999999645 ) ) ;
#18881 = CARTESIAN_POINT ( 'NONE',  ( 69.85000000109246798, 9.999999999999998224, 17.06698730000000097 ) ) ;
#18882 = ADVANCED_FACE ( 'NONE', ( #19106 ), #2697, .F. ) ;
#18883 = PRODUCT_DEFINITION_SHAPE ( 'NONE', 'NONE',  #23704 ) ;
#18884 = ORIENTED_EDGE ( 'NONE', *, *, #1261, .F. ) ;
#18885 = CARTESIAN_POINT ( 'NONE',  ( 24.42673246966726452, -11.25000000000000355, 5.000000000000079936 ) ) ;
#18886 = CARTESIAN_POINT ( 'NONE',  ( 53.71875000000002132, 14.00000000000000888, 16.65685424949235482 ) ) ;
#18887 = CARTESIAN_POINT ( 'NONE',  ( 118.3095189484530181, -14.69846310392956745, 35.82846581308617573 ) ) ;
#18888 = EDGE_CURVE ( 'NONE', #10460, #6517, #23117, .T. ) ;
#18889 = CARTESIAN_POINT ( 'NONE',  ( 66.75000000218494733, 12.50000000000000000, 13.96446609406725692 ) ) ;
#18890 = CARTESIAN_POINT ( 'NONE',  ( 32.13446180928345086, -8.974600000000002353, 5.000000000000079936 ) ) ;
#18891 = ADVANCED_FACE ( 'NONE', ( #11954 ), #19223, .F. ) ;
#18892 = CARTESIAN_POINT ( 'NONE',  ( -66.65000000109247935, 9.999999999999998224, 17.06698730000000097 ) ) ;
#18893 = ORIENTED_EDGE ( 'NONE', *, *, #19317, .T. ) ;
#18894 = PLANE ( 'NONE',  #10748 ) ;
#18895 = EDGE_LOOP ( 'NONE', ( #6903, #16393, #17276, #13189 ) ) ;
#18896 = CARTESIAN_POINT ( 'NONE',  ( 33.85151041966726382, -11.25000000000000355, 5.000000000000079936 ) ) ;
#18897 = DIRECTION ( 'NONE',  ( 0.000000000000000000, 0.000000000000000000, -1.000000000000000000 ) ) ;
#18898 = EDGE_LOOP ( 'NONE', ( #13781, #6250, #9092, #15963 ) ) ;
#18899 = CARTESIAN_POINT ( 'NONE',  ( -4.000000000000000000, 2.309401076758498483, -0.4999999999999927280 ) ) ;
#18900 = CARTESIAN_POINT ( 'NONE',  ( 15.82088754676620823, -9.000000000000003553, 5.000000000000079936 ) ) ;
#18901 = CARTESIAN_POINT ( 'NONE',  ( 1.971781867644420635E-15, -4.000000000000000000, 11.37500000273119660 ) ) ;
#18902 = CYLINDRICAL_SURFACE ( 'NONE', #5253, 4.000000000000001776 ) ;
#18903 = ORIENTED_EDGE ( 'NONE', *, *, #12326, .T. ) ;
#18904 = CARTESIAN_POINT ( 'NONE',  ( 3.802871176606126280, 5.309964801958114045, -3.686277791023383266 ) ) ;
#18905 = ORIENTED_EDGE ( 'NONE', *, *, #3074, .T. ) ;
#18906 = CARTESIAN_POINT ( 'NONE',  ( 71.05000000109247082, 12.06698730000000097, 14.99999999999999645 ) ) ;
#18907 = CARTESIAN_POINT ( 'NONE',  ( -2.828427124746188515, -2.828427124746190735, 15.12500000000001066 ) ) ;
#18908 = CARTESIAN_POINT ( 'NONE',  ( 4.999999999999999112, 0.000000000000000000, 0.000000000000000000 ) ) ;
#18909 = CARTESIAN_POINT ( 'NONE',  ( 0.000000000000000000, 0.000000000000000000, 19.04999999999996874 ) ) ;
#18910 = DIRECTION ( 'NONE',  ( -1.000000000000000000, -0.000000000000000000, -0.000000000000000000 ) ) ;
#18911 = CARTESIAN_POINT ( 'NONE',  ( 69.15000000109246514, 8.538419263543522320, 16.46158073645647235 ) ) ;
#18912 = ORIENTED_EDGE ( 'NONE', *, *, #13020, .F. ) ;
#18913 = LINE ( 'NONE', #2619, #2232 ) ;
#18914 = CYLINDRICAL_SURFACE ( 'NONE', #21346, 4.000000000000001776 ) ;
#18915 = EDGE_CURVE ( 'NONE', #21207, #2537, #18133, .T. ) ;
#18916 = CARTESIAN_POINT ( 'NONE',  ( 70.35000000109246798, 11.46158073645647235, 13.53841926354352232 ) ) ;
#18917 = CARTESIAN_POINT ( 'NONE',  ( 2.445694354108821855, -2.445694354108820079, 12.81250000136560629 ) ) ;
#18918 = VECTOR ( 'NONE', #10885, 1000.000000000000000 ) ;
#18919 = FACE_OUTER_BOUND ( 'NONE', #11462, .T. ) ;
#18920 = EDGE_CURVE ( 'NONE', #22617, #5234, #23642, .T. ) ;
#18921 = AXIS2_PLACEMENT_3D ( 'NONE', #16119, #1599, #12180 ) ;
#18922 = CARTESIAN_POINT ( 'NONE',  ( 4.999999999999999112, 8.461683424509345741, -2.223716399045483350 ) ) ;
#18923 = ORIENTED_EDGE ( 'NONE', *, *, #17291, .F. ) ;
#18924 = CARTESIAN_POINT ( 'NONE',  ( 2.828427124746190735, -2.828427124746189847, 0.6750000000000020428 ) ) ;
#18925 = CARTESIAN_POINT ( 'NONE',  ( -90.00000000000000000, 0.000000000000000000, 0.000000000000000000 ) ) ;
#18926 = AXIS2_PLACEMENT_3D ( 'NONE', #19994, #11051, #22021 ) ;
#18927 = CARTESIAN_POINT ( 'NONE',  ( 2.445694354108821411, 2.445694354108820523, 11.06250000136560452 ) ) ;
#18928 = DIRECTION ( 'NONE',  ( -1.000000000000000000, 0.000000000000000000, 0.000000000000000000 ) ) ;
#18929 = ORIENTED_EDGE ( 'NONE', *, *, #9100, .T. ) ;
#18930 = CARTESIAN_POINT ( 'NONE',  ( -65.65000000109247935, 9.999999999999998224, 17.06698730000000097 ) ) ;
#18931 = ORIENTED_EDGE ( 'NONE', *, *, #7963, .T. ) ;
#18932 = CARTESIAN_POINT ( 'NONE',  ( 52.37268183416157541, 7.219692298483935566, 12.12345345202367675 ) ) ;
#18933 = CARTESIAN_POINT ( 'NONE',  ( -68.65000000109246514, 9.999999999999998224, 12.93301269999999192 ) ) ;
#18934 = CONTEXT_DEPENDENT_SHAPE_REPRESENTATION ( #22621, #20395 ) ;
#18935 = ORIENTED_EDGE ( 'NONE', *, *, #15650, .F. ) ;
#18936 = LINE ( 'NONE', #4681, #7110 ) ;
#18937 = ORIENTED_EDGE ( 'NONE', *, *, #2005, .T. ) ;
#18938 = ORIENTED_EDGE ( 'NONE', *, *, #16683, .T. ) ;
#18939 = CARTESIAN_POINT ( 'NONE',  ( 2.445694354108821411, 2.445694354108820523, 18.31250000136560274 ) ) ;
#18940 = CARTESIAN_POINT ( 'NONE',  ( 58.21875000000000711, 13.00000000000000711, 16.24264068711927322 ) ) ;
#18941 = AXIS2_PLACEMENT_3D ( 'NONE', #4648, #8698, #23409 ) ;
#18942 = CARTESIAN_POINT ( 'NONE',  ( -67.00000000109247367, 12.06698730000000275, 14.14382582708705094 ) ) ;
#18943 = CIRCLE ( 'NONE', #8633, 4.999999999999997335 ) ;
#18944 = CARTESIAN_POINT ( 'NONE',  ( 68.85000000109248219, 9.999999999999998224, 17.06698730000000097 ) ) ;
#18945 = CARTESIAN_POINT ( 'NONE',  ( -67.65000000109247935, 7.933012699999995476, 14.99999999999999645 ) ) ;
#18946 = CARTESIAN_POINT ( 'NONE',  ( 58.93518183416157541, 9.931948859054372747, 17.99999999999999645 ) ) ;
#18947 = CARTESIAN_POINT ( 'NONE',  ( -15.00000000000000711, 10.00000000000000000, -19.99999999999999645 ) ) ;
#18948 = CARTESIAN_POINT ( 'NONE',  ( -1.432654583217640498, 3.458734125000000770, 4.800000001365595459 ) ) ;
#18949 = CARTESIAN_POINT ( 'NONE',  ( -1.432654583217638944, 3.458734125000000326, 11.25000000136560452 ) ) ;
#18950 = CARTESIAN_POINT ( 'NONE',  ( 1.656854249492384135, -3.999999999999999112, 11.43750000273119660 ) ) ;
#18951 = LINE ( 'NONE', #23019, #20652 ) ;
#18952 = VERTEX_POINT ( 'NONE', #23161 ) ;
#18953 = CARTESIAN_POINT ( 'NONE',  ( 12.68853974071656232, -8.974600000000002353, 5.000000000000079936 ) ) ;
#18954 = ORIENTED_EDGE ( 'NONE', *, *, #23224, .F. ) ;
#18955 = CARTESIAN_POINT ( 'NONE',  ( 56.68518183416157541, 10.06805114094562548, 11.99999999999999645 ) ) ;
#18956 = AXIS2_PLACEMENT_3D ( 'NONE', #7841, #18375, #407 ) ;
#18957 = CARTESIAN_POINT ( 'NONE',  ( 2.445694354108820523, -2.445694354108820079, 2.112500001365596791 ) ) ;
#18958 = PRODUCT_DEFINITION ( 'UNKNOWN', '', #14909, #13653 ) ;
#18959 = VECTOR ( 'NONE', #18394, 1000.000000000000000 ) ;
#18960 = FACE_OUTER_BOUND ( 'NONE', #9322, .T. ) ;
#18961 = ORIENTED_EDGE ( 'NONE', *, *, #21834, .T. ) ;
#18962 = CARTESIAN_POINT ( 'NONE',  ( -1.656854249492379250, 4.000000000000000000, 14.81250000000001066 ) ) ;
#18963 = ADVANCED_FACE ( 'NONE', ( #3405, #1711 ), #15883, .F. ) ;
#18964 = LINE ( 'NONE', #18847, #4124 ) ;
#18965 = DIRECTION ( 'NONE',  ( -1.000000000000000000, 0.000000000000000000, 9.637352644315595243E-17 ) ) ;
#18966 = ORIENTED_EDGE ( 'NONE', *, *, #424, .F. ) ;
#18967 = CARTESIAN_POINT ( 'NONE',  ( -70.20000000218495018, 9.999999999999998224, 17.49999999999999645 ) ) ;
#18968 = CARTESIAN_POINT ( 'NONE',  ( 3.458734125000001214, -1.432654583217639610, -1.574999998634403875 ) ) ;
#18969 = CARTESIAN_POINT ( 'NONE',  ( -4.101948962585905356, -2.368261337751088824, -3.681124513963624167 ) ) ;
#18970 = CARTESIAN_POINT ( 'NONE',  ( 1.432654583217641386, 3.458734125000000770, 18.37500000136560629 ) ) ;
#18971 = DIRECTION ( 'NONE',  ( 1.000000000000000000, 7.703719777548943412E-32, 0.000000000000000000 ) ) ;
#18972 = CARTESIAN_POINT ( 'NONE',  ( 71.15000000109247935, 11.46158073645647235, 16.46158073645647235 ) ) ;
#18973 = FACE_OUTER_BOUND ( 'NONE', #7234, .T. ) ;
#18974 = CARTESIAN_POINT ( 'NONE',  ( 56.75231816583843170, 7.926799079670502124, 17.16943976678978245 ) ) ;
#18975 = CARTESIAN_POINT ( 'NONE',  ( 2.445694354108820079, 2.445694354108820523, 3.612500001365598123 ) ) ;
#18976 = CARTESIAN_POINT ( 'NONE',  ( -2.445694354108818303, -2.445694354108820967, 10.81250000136560452 ) ) ;
#18977 = CARTESIAN_POINT ( 'NONE',  ( -20.00005080000000035, 7.347880794884120722E-16, 6.000000000000000888 ) ) ;
#18978 = DIRECTION ( 'NONE',  ( 1.000000000000000000, 7.703719777548943412E-32, 0.000000000000000000 ) ) ;
#18979 = LINE ( 'NONE', #9911, #13976 ) ;
#18980 = ORIENTED_EDGE ( 'NONE', *, *, #22727, .F. ) ;
#18981 = CARTESIAN_POINT ( 'NONE',  ( -3.455068668934486276, 2.624017327439035707, -3.316620875263955437 ) ) ;
#18982 = CARTESIAN_POINT ( 'NONE',  ( -4.000000000000000888, 1.656854249492380804, 3.362500002731190651 ) ) ;
#18983 = CARTESIAN_POINT ( 'NONE',  ( -69.60000000109249640, 10.85617417291294551, 17.06698729999999742 ) ) ;
#18984 = ORIENTED_EDGE ( 'NONE', *, *, #21156, .F. ) ;
#18985 = ORIENTED_EDGE ( 'NONE', *, *, #11193, .F. ) ;
#18986 = EDGE_CURVE ( 'NONE', #15433, #20420, #4001, .T. ) ;
#18987 = CARTESIAN_POINT ( 'NONE',  ( -0.3198814748697807464, -4.434118497892185040, -0.3507732604232532969 ) ) ;
#18988 = EDGE_CURVE ( 'NONE', #12095, #18227, #12069, .T. ) ;
#18989 = CARTESIAN_POINT ( 'NONE',  ( 52.78125000000000000, 8.343145750507600766, 11.00000000000000355 ) ) ;
#18990 = VERTEX_POINT ( 'NONE', #10750 ) ;
#18991 = DIRECTION ( 'NONE',  ( 1.000000000000000000, 0.000000000000000000, 0.000000000000000000 ) ) ;
#18992 = ADVANCED_FACE ( 'NONE', ( #12665 ), #18023, .T. ) ;
#18993 = CARTESIAN_POINT ( 'NONE',  ( 67.40000000109247935, 7.933012699999995476, 15.85617417291294196 ) ) ;
#18994 = CARTESIAN_POINT ( 'NONE',  ( 69.70000000109246230, 12.06698730000000275, 15.85617417291294196 ) ) ;
#18995 = VERTEX_POINT ( 'NONE', #14086 ) ;
#18996 = VECTOR ( 'NONE', #13972, 1000.000000000000000 ) ;
#18997 = DIRECTION ( 'NONE',  ( -0.000000000000000000, -0.000000000000000000, 1.000000000000000000 ) ) ;
#18998 = CARTESIAN_POINT ( 'NONE',  ( 57.65625000000002132, 6.000000000000004441, 16.65685424949239390 ) ) ;
#18999 = DIRECTION ( 'NONE',  ( 1.000000000000000000, 0.000000000000000000, 0.000000000000000000 ) ) ;
#19000 = CARTESIAN_POINT ( 'NONE',  ( -3.458734124999998105, -1.432654583217642275, 18.50000000136560629 ) ) ;
#19001 = CARTESIAN_POINT ( 'NONE',  ( 0.000000000000000000, -5.222868219166923787, 9.680994141368751471 ) ) ;
#19002 = DIRECTION ( 'NONE',  ( -1.000000000000000000, 0.000000000000000000, 0.000000000000000000 ) ) ;
#19003 = VERTEX_POINT ( 'NONE', #3160 ) ;
#19004 = CARTESIAN_POINT ( 'NONE',  ( 8.673617379884035472E-16, 4.618802153517012954, -5.000000000000000000 ) ) ;
#19005 =( BOUNDED_SURFACE ( )  B_SPLINE_SURFACE ( 1, 2, ( 
 ( #12204, #23309, #2828, #12437, #8597, #12087, #1149, #17466, #17583, #17923, #4997, #23428, #16020, #10417, #19476, #23180, #19352, #16142, #2941, #15903, #3305, #8365, #1508, #3073, #13990, #12325, #21252, #1030, #17697, #3184, #21492, #7034, #21612, #8490, #19588, #13880, #10530, #17808, #15683, #22956, #6918, #14352, #10294, #5219, #12564, #10648, #6564, #1258, #14236, #4869, #1376, #21138, #4751, #15794, #6791, #23066, #14112, #8714, #21375, #5105, #5576, #13029, #7629, #18045, #18156, #23545, #1622, #10771, #3771, #21733, #16487, #18389, #20049, #9077, #16599, #5694, #5460, #12796, #14823, #7153, #14707, #5814, #20289, #19824, #14951, #11111, #16715, #293, #16255, #18500, #2086, #22203, #3430, #16368, #22076, #23664, #14467, #7395, #3890, #3653, #12904, #20164, #8965, #5345, #7510, #12689, #1969, #19943, #9309, #3543, #179, #21964, #11226, #9426, #10878, #1738, #7281, #14594, #21854, #10988, #18267, #1852, #9201, #63, #15181, #9781, #422, #11708, #8112, #22803, #17076, #15065, #15539, #4013, #13385, #13614, #20876, #11350, #11475, #6181, #15421, #779, #4133, #13141, #19100, #20405, #11593, #2558, #6297 ),
 ( #18861, #22685, #2692, #4485, #650, #9906, #7983, #17320, #22320, #17201, #11825, #10032, #2446, #886, #18751, #2335, #8221, #7749, #20654, #18622, #2209, #13501, #9548, #16845, #5936, #20525, #9668, #13262, #16958, #535, #4258, #6053, #15303, #22440, #7858, #22577, #20766, #4369, #18975, #16114, #12174, #13856, #20996, #4616, #8466, #1005, #8816, #21228, #2805, #17671, #12299, #8337, #10265, #4728, #15770, #8687, #17780, #1232, #19444, #12060, #1121, #10501, #6765, #6654, #1473, #15878, #8571, #14207, #19561, #21344, #6886, #15992, #5077, #19215, #21464, #10146, #19327, #3155, #23276, #23042, #3041, #17440, #4968, #1353, #6417, #10390, #15655, #13732, #11950, #13966, #12409, #19674, #22927, #2915, #23154, #3280, #10622, #21111, #6540, #17896, #17555, #4840, #14081, #16907, #18565, #19918, #9617, #2278, #5194, #5766, #485, #5996, #7808, #20349, #20470, #2148, #4198, #8933, #13204, #22386, #4076, #13094, #13323, #21706, #12657, #18689, #18018, #7570, #20592, #14321, #363, #11541, #9726, #1594, #7126, #5315, #18810, #2393, #3396, #236, #16661, #3956, #2030, #21580, #11290, #22147, #23398, #9483, #7002 ) ),
 .UNSPECIFIED., .F., .F., .F. ) 
 B_SPLINE_SURFACE_WITH_KNOTS ( ( 2, 2 ),
 ( 3, 2, 2, 2, 2, 2, 2, 2, 2, 2, 2, 2, 2, 2, 2, 2, 2, 2, 2, 2, 2, 2, 2, 2, 2, 2, 2, 2, 2, 2, 2, 2, 2, 2, 2, 2, 2, 2, 2, 2, 2, 2, 2, 2, 2, 2, 2, 2, 2, 2, 2, 2, 2, 2, 2, 2, 2, 2, 2, 2, 2, 2, 2, 2, 2, 2, 2, 2, 2, 2, 2, 2, 2, 2, 3 ),
 ( 0.000000000000000000, 1.000000000000000000 ),
 ( 0.000000000000000000, 0.01250000000000000069, 0.02500000000000000139, 0.03749999999999999861, 0.05000000000000000278, 0.06250000000000000000, 0.07499999999999999722, 0.08749999999999999445, 0.1000000000000000056, 0.1125000000000000028, 0.1250000000000000000, 0.1375000000000000111, 0.1499999999999999944, 0.1625000000000000056, 0.1749999999999999889, 0.1875000000000000000, 0.2000000000000000111, 0.2124999999999999944, 0.2250000000000000056, 0.2374999999999999889, 0.2500000000000000000, 0.2625000000000000111, 0.2750000000000000222, 0.2874999999999999778, 0.2999999999999999889, 0.3125000000000000000, 0.3250000000000000111, 0.3375000000000000222, 0.3499999999999999778, 0.3624999999999999889, 0.3750000000000000000, 0.3875000000000000111, 0.4000000000000000222, 0.4124999999999999778, 0.4249999999999999889, 0.4375000000000000000, 0.4500000000000000111, 0.4625000000000000222, 0.4749999999999999778, 0.4874999999999999889, 0.5000000000000000000, 0.5124999999999999556, 0.5250000000000000222, 0.5374999999999999778, 0.5500000000000000444, 0.5625000000000000000, 0.5749999999999999556, 0.5875000000000000222, 0.5999999999999999778, 0.6125000000000000444, 0.6250000000000000000, 0.6374999999999999556, 0.6500000000000000222, 0.6624999999999999778, 0.6750000000000000444, 0.6875000000000000000, 0.6999999999999999556, 0.7125000000000000222, 0.7249999999999999778, 0.7375000000000000444, 0.7500000000000000000, 0.7624999999999999556, 0.7750000000000000222, 0.7874999999999999778, 0.8000000000000000444, 0.8125000000000000000, 0.8249999999999999556, 0.8375000000000000222, 0.8499999999999999778, 0.8625000000000000444, 0.8750000000000000000, 0.8874999999999999556, 0.9000000000000000222, 0.9124999999999999778, 0.9250000000000000444 ),
 .UNSPECIFIED. ) 
 GEOMETRIC_REPRESENTATION_ITEM ( )  RATIONAL_B_SPLINE_SURFACE ( (
 ( 1.000000000000000000, 0.9238795325112867385, 1.000000000000000000, 0.9238795325112867385, 1.000000000000000000, 0.9238795325112867385, 1.000000000000000000, 0.9238795325112867385, 1.000000000000000000, 0.9238795325112867385, 1.000000000000000000, 0.9238795325112867385, 1.000000000000000000, 0.9238795325112867385, 1.000000000000000000, 0.9238795325112867385, 1.000000000000000000, 0.9238795325112867385, 1.000000000000000000, 0.9238795325112867385, 1.000000000000000000, 0.9238795325112867385, 1.000000000000000000, 0.9238795325112867385, 1.000000000000000000, 0.9238795325112867385, 1.000000000000000000, 0.9238795325112867385, 1.000000000000000000, 0.9238795325112867385, 1.000000000000000000, 0.9238795325112867385, 1.000000000000000000, 0.9238795325112867385, 1.000000000000000000, 0.9238795325112867385, 1.000000000000000000, 0.9238795325112867385, 1.000000000000000000, 0.9238795325112867385, 1.000000000000000000, 0.9238795325112867385, 1.000000000000000000, 0.9238795325112867385, 1.000000000000000000, 0.9238795325112867385, 1.000000000000000000, 0.9238795325112867385, 1.000000000000000000, 0.9238795325112867385, 1.000000000000000000, 0.9238795325112867385, 1.000000000000000000, 0.9238795325112867385, 1.000000000000000000, 0.9238795325112867385, 1.000000000000000000, 0.9238795325112867385, 1.000000000000000000, 0.9238795325112867385, 1.000000000000000000, 0.9238795325112867385, 1.000000000000000000, 0.9238795325112867385, 1.000000000000000000, 0.9238795325112867385, 1.000000000000000000, 0.9238795325112867385, 1.000000000000000000, 0.9238795325112867385, 1.000000000000000000, 0.9238795325112867385, 1.000000000000000000, 0.9238795325112867385, 1.000000000000000000, 0.9238795325112867385, 1.000000000000000000, 0.9238795325112867385, 1.000000000000000000, 0.9238795325112867385, 1.000000000000000000, 0.9238795325112867385, 1.000000000000000000, 0.9238795325112867385, 1.000000000000000000, 0.9238795325112867385, 1.000000000000000000, 0.9238795325112867385, 1.000000000000000000, 0.9238795325112867385, 1.000000000000000000, 0.9238795325112867385, 1.000000000000000000, 0.9238795325112867385, 1.000000000000000000, 0.9238795325112867385, 1.000000000000000000, 0.9238795325112867385, 1.000000000000000000, 0.9238795325112867385, 1.000000000000000000, 0.9238795325112867385, 1.000000000000000000, 0.9238795325112867385, 1.000000000000000000, 0.9238795325112867385, 1.000000000000000000, 0.9238795325112867385, 1.000000000000000000, 0.9238795325112867385, 1.000000000000000000, 0.9238795325112867385, 1.000000000000000000, 0.9238795325112867385, 1.000000000000000000, 0.9238795325112867385, 1.000000000000000000, 0.9238795325112867385, 1.000000000000000000, 0.9238795325112867385, 1.000000000000000000, 0.9238795325112867385, 1.000000000000000000, 0.9238795325112867385, 1.000000000000000000, 0.9238795325112867385, 1.000000000000000000, 0.9238795325112867385, 1.000000000000000000, 0.9238795325112867385, 1.000000000000000000, 0.9238795325112867385, 1.000000000000000000, 0.9238795325112867385, 1.000000000000000000, 0.9238795325112867385, 1.000000000000000000, 0.9238795325112867385, 1.000000000000000000, 0.9238795325112867385, 1.000000000000000000, 0.9238795325112867385, 1.000000000000000000, 0.9238795325112867385, 1.000000000000000000, 0.9238795325112867385, 1.000000000000000000, 0.9238795325112867385, 1.000000000000000000),
 ( 1.000000000000000000, 0.9238795325112867385, 1.000000000000000000, 0.9238795325112867385, 1.000000000000000000, 0.9238795325112867385, 1.000000000000000000, 0.9238795325112867385, 1.000000000000000000, 0.9238795325112867385, 1.000000000000000000, 0.9238795325112867385, 1.000000000000000000, 0.9238795325112867385, 1.000000000000000000, 0.9238795325112867385, 1.000000000000000000, 0.9238795325112867385, 1.000000000000000000, 0.9238795325112867385, 1.000000000000000000, 0.9238795325112867385, 1.000000000000000000, 0.9238795325112867385, 1.000000000000000000, 0.9238795325112867385, 1.000000000000000000, 0.9238795325112867385, 1.000000000000000000, 0.9238795325112867385, 1.000000000000000000, 0.9238795325112867385, 1.000000000000000000, 0.9238795325112867385, 1.000000000000000000, 0.9238795325112867385, 1.000000000000000000, 0.9238795325112867385, 1.000000000000000000, 0.9238795325112867385, 1.000000000000000000, 0.9238795325112867385, 1.000000000000000000, 0.9238795325112867385, 1.000000000000000000, 0.9238795325112867385, 1.000000000000000000, 0.9238795325112867385, 1.000000000000000000, 0.9238795325112867385, 1.000000000000000000, 0.9238795325112867385, 1.000000000000000000, 0.9238795325112867385, 1.000000000000000000, 0.9238795325112867385, 1.000000000000000000, 0.9238795325112867385, 1.000000000000000000, 0.9238795325112867385, 1.000000000000000000, 0.9238795325112867385, 1.000000000000000000, 0.9238795325112867385, 1.000000000000000000, 0.9238795325112867385, 1.000000000000000000, 0.9238795325112867385, 1.000000000000000000, 0.9238795325112867385, 1.000000000000000000, 0.9238795325112867385, 1.000000000000000000, 0.9238795325112867385, 1.000000000000000000, 0.9238795325112867385, 1.000000000000000000, 0.9238795325112867385, 1.000000000000000000, 0.9238795325112867385, 1.000000000000000000, 0.9238795325112867385, 1.000000000000000000, 0.9238795325112867385, 1.000000000000000000, 0.9238795325112867385, 1.000000000000000000, 0.9238795325112867385, 1.000000000000000000, 0.9238795325112867385, 1.000000000000000000, 0.9238795325112867385, 1.000000000000000000, 0.9238795325112867385, 1.000000000000000000, 0.9238795325112867385, 1.000000000000000000, 0.9238795325112867385, 1.000000000000000000, 0.9238795325112867385, 1.000000000000000000, 0.9238795325112867385, 1.000000000000000000, 0.9238795325112867385, 1.000000000000000000, 0.9238795325112867385, 1.000000000000000000, 0.9238795325112867385, 1.000000000000000000, 0.9238795325112867385, 1.000000000000000000, 0.9238795325112867385, 1.000000000000000000, 0.9238795325112867385, 1.000000000000000000, 0.9238795325112867385, 1.000000000000000000, 0.9238795325112867385, 1.000000000000000000, 0.9238795325112867385, 1.000000000000000000, 0.9238795325112867385, 1.000000000000000000, 0.9238795325112867385, 1.000000000000000000, 0.9238795325112867385, 1.000000000000000000, 0.9238795325112867385, 1.000000000000000000, 0.9238795325112867385, 1.000000000000000000, 0.9238795325112867385, 1.000000000000000000, 0.9238795325112867385, 1.000000000000000000, 0.9238795325112867385, 1.000000000000000000, 0.9238795325112867385, 1.000000000000000000, 0.9238795325112867385, 1.000000000000000000, 0.9238795325112867385, 1.000000000000000000, 0.9238795325112867385, 1.000000000000000000, 0.9238795325112867385, 1.000000000000000000, 0.9238795325112867385, 1.000000000000000000) ) ) 
 REPRESENTATION_ITEM ( '' )  SURFACE ( )  );
#19006 = CARTESIAN_POINT ( 'NONE',  ( -7.000000000000000000, 8.572527594031473190E-16, 1.734723475976807094E-15 ) ) ;
#19007 = CARTESIAN_POINT ( 'NONE',  ( 5.577176569667260608, -11.25000000000000355, 5.000000000000079936 ) ) ;
#19008 = CIRCLE ( 'NONE', #8708, 11.00000000000000000 ) ;
#19009 = VERTEX_POINT ( 'NONE', #8577 ) ;
#19010 = CARTESIAN_POINT ( 'NONE',  ( 69.20000000218495018, 12.50000000000000000, 14.99999999999999645 ) ) ;
#19011 = ADVANCED_FACE ( 'NONE', ( #19566 ), #23517, .T. ) ;
#19012 = DIRECTION ( 'NONE',  ( -0.000000000000000000, 1.000000000000000000, -0.000000000000000000 ) ) ;
#19013 = CARTESIAN_POINT ( 'NONE',  ( -1.800000000000000711, 0.000000000000000000, -6.200000000000020606 ) ) ;
#19014 = EDGE_CURVE ( 'NONE', #3575, #17091, #21234, .T. ) ;
#19015 = CARTESIAN_POINT ( 'NONE',  ( -1.520000000000000462, 0.000000000000000000, 0.000000000000000000 ) ) ;
#19016 = VERTEX_POINT ( 'NONE', #12414 ) ;
#19017 = CARTESIAN_POINT ( 'NONE',  ( -20.00000000000000711, 9.999999999999964473, -19.99999999999999645 ) ) ;
#19018 = VERTEX_POINT ( 'NONE', #21351 ) ;
#19019 = CARTESIAN_POINT ( 'NONE',  ( 9.920644283265380691E-16, 4.000000000000000000, 17.75000000000000711 ) ) ;
#19020 = CARTESIAN_POINT ( 'NONE',  ( 31.52885079676620705, -9.000000000000003553, 5.000000000000079936 ) ) ;
#19021 = EDGE_CURVE ( 'NONE', #8937, #16346, #6892, .T. ) ;
#19022 = CARTESIAN_POINT ( 'NONE',  ( -8.706242640716551406, -8.974600000000002353, 5.000000000000079936 ) ) ;
#19023 = EDGE_CURVE ( 'NONE', #22160, #19814, #4769, .T. ) ;
#19024 = AXIS2_PLACEMENT_3D ( 'NONE', #4831, #12963, #1343 ) ;
#19025 = ORIENTED_EDGE ( 'NONE', *, *, #4889, .F. ) ;
#19026 = DIRECTION ( 'NONE',  ( 1.000000000000000000, 0.000000000000000000, 0.000000000000000000 ) ) ;
#19027 = ADVANCED_BREP_SHAPE_REPRESENTATION ( '', ( #21929, #7318 ), #13013 ) ;
#19028 = LINE ( 'NONE', #4658, #12188 ) ;
#19029 = CARTESIAN_POINT ( 'NONE',  ( 67.25000000109245946, 12.06698730000000097, 14.99999999999999645 ) ) ;
#19030 = ORIENTED_EDGE ( 'NONE', *, *, #20329, .T. ) ;
#19031 = AXIS2_PLACEMENT_3D ( 'NONE', #6522, #2899, #21097 ) ;
#19032 = CARTESIAN_POINT ( 'NONE',  ( 12.67929489676620314, -9.000000000000003553, 5.000000000000079936 ) ) ;
#19033 = CARTESIAN_POINT ( 'NONE',  ( 4.000000000000001776, -1.656854249492379694, 10.56250000273119660 ) ) ;
#19034 = CARTESIAN_POINT ( 'NONE',  ( 70.90000000109245093, 7.933012699999995476, 14.14382582708705094 ) ) ;
#19035 = CARTESIAN_POINT ( 'NONE',  ( 1.432654583217643163, -3.458734124999999437, 13.75000000136560452 ) ) ;
#19036 = CARTESIAN_POINT ( 'NONE',  ( 0.000000000000000000, 1.975651141462237970, 10.82112760146736896 ) ) ;
#19037 = PLANE ( 'NONE',  #5396 ) ;
#19038 = ORIENTED_EDGE ( 'NONE', *, *, #20915, .T. ) ;
#19039 = CARTESIAN_POINT ( 'NONE',  ( 4.000000000000000000, 1.656854249492381248, 2.862500000000002043 ) ) ;
#19040 = CARTESIAN_POINT ( 'NONE',  ( 4.999999999999999112, 6.807171995660585395, 6.478011392632914145 ) ) ;
#19041 = CARTESIAN_POINT ( 'NONE',  ( -3.458734124999998993, -1.432654583217642497, 11.50000000136560629 ) ) ;
#19042 = CARTESIAN_POINT ( 'NONE',  ( 4.999999999999999112, 1.699438267350372067, 9.241976615262164074 ) ) ;
#19043 = ORIENTED_EDGE ( 'NONE', *, *, #110, .T. ) ;
#19044 = AXIS2_PLACEMENT_3D ( 'NONE', #19984, #3587, #10925 ) ;
#19045 = CARTESIAN_POINT ( 'NONE',  ( 0.000000000000000000, 3.174628368996076588, 8.152713396088772768 ) ) ;
#19046 = ORIENTED_EDGE ( 'NONE', *, *, #18463, .F. ) ;
#19047 = CARTESIAN_POINT ( 'NONE',  ( -66.60000000109246798, 10.85617417291294551, 17.06698729999999742 ) ) ;
#19048 = CONTEXT_DEPENDENT_SHAPE_REPRESENTATION ( #5169, #8005 ) ;
#19049 = EDGE_CURVE ( 'NONE', #15450, #8473, #14445, .T. ) ;
#19050 = ORIENTED_EDGE ( 'NONE', *, *, #6001, .F. ) ;
#19051 = DIRECTION ( 'NONE',  ( 0.000000000000000000, 0.000000000000000000, -1.000000000000000000 ) ) ;
#19052 = ORIENTED_EDGE ( 'NONE', *, *, #21829, .F. ) ;
#19053 = AXIS2_PLACEMENT_3D ( 'NONE', #53, #20279, #20036 ) ;
#19054 = ADVANCED_FACE ( 'NONE', ( #10856 ), #7287, .F. ) ;
#19055 =( GEOMETRIC_REPRESENTATION_CONTEXT ( 3 ) GLOBAL_UNCERTAINTY_ASSIGNED_CONTEXT ( ( #9798 ) ) GLOBAL_UNIT_ASSIGNED_CONTEXT ( ( #11687, #20744, #22303 ) ) REPRESENTATION_CONTEXT ( 'NONE', 'WORKASPACE' ) );
#19056 = ORIENTED_EDGE ( 'NONE', *, *, #13216, .T. ) ;
#19057 = CARTESIAN_POINT ( 'NONE',  ( -1.432654583217639166, 3.458734125000000770, 17.50000000136560274 ) ) ;
#19058 = CARTESIAN_POINT ( 'NONE',  ( -2.449293598294706907E-16, 4.000000000000000000, -3.674599999999999866 ) ) ;
#19059 = EDGE_CURVE ( 'NONE', #9354, #20516, #17020, .T. ) ;
#19060 = CARTESIAN_POINT ( 'NONE',  ( -68.45000000109247651, 9.999999999999998224, 12.93301269999999192 ) ) ;
#19061 = CARTESIAN_POINT ( 'NONE',  ( 69.50000000109247367, 12.06698729999999919, 15.85617417291294196 ) ) ;
#19062 = CIRCLE ( 'NONE', #9144, 4.000000000000001776 ) ;
#19063 = CARTESIAN_POINT ( 'NONE',  ( -67.05000000109247082, 9.999999999999998224, 12.93301269999999192 ) ) ;
#19064 = CYLINDRICAL_SURFACE ( 'NONE', #2293, 11.00000000000000000 ) ;
#19065 = CARTESIAN_POINT ( 'NONE',  ( 58.27893183416158962, 8.825410453826341595, 11.97181229448535511 ) ) ;
#19066 = PLANE ( 'NONE',  #11244 ) ;
#19067 = AXIS2_PLACEMENT_3D ( 'NONE', #3085, #7045, #21505 ) ;
#19068 = AXIS2_PLACEMENT_3D ( 'NONE', #21509, #17480, #3089 ) ;
#19069 = CARTESIAN_POINT ( 'NONE',  ( -3.458734125000000770, 1.432654583217640498, 1.925000001365597457 ) ) ;
#19070 = CARTESIAN_POINT ( 'NONE',  ( 71.50000000000000000, 12.50000000000000000, 14.99999999999999645 ) ) ;
#19071 = CARTESIAN_POINT ( 'NONE',  ( -1.656854249492380138, -3.999999999999999112, 10.31250000273119483 ) ) ;
#19072 = DIRECTION ( 'NONE',  ( -1.000000000000000000, -0.000000000000000000, -0.000000000000000000 ) ) ;
#19073 = ORIENTED_EDGE ( 'NONE', *, *, #10920, .T. ) ;
#19074 = DIRECTION ( 'NONE',  ( 1.000000000000000000, 7.703719777548943412E-32, 0.000000000000000000 ) ) ;
#19075 = VERTEX_POINT ( 'NONE', #401 ) ;
#19076 = CARTESIAN_POINT ( 'NONE',  ( 55.65393183416158251, 6.971812294485357775, 16.17458954617365663 ) ) ;
#19077 = DIRECTION ( 'NONE',  ( 0.000000000000000000, 0.000000000000000000, 1.000000000000000000 ) ) ;
#19078 = CARTESIAN_POINT ( 'NONE',  ( 2.445694354108820079, 2.445694354108820523, 1.362500001365595903 ) ) ;
#19079 = VECTOR ( 'NONE', #10443, 1000.000000000000114 ) ;
#19080 = CARTESIAN_POINT ( 'NONE',  ( -2.445694354108819635, -2.445694354108820523, -1.137499998634402765 ) ) ;
#19081 = VERTEX_POINT ( 'NONE', #515 ) ;
#19082 = LINE ( 'NONE', #17304, #20950 ) ;
#19083 = CARTESIAN_POINT ( 'NONE',  ( 4.999999999999999112, 2.223716399045570835, 8.461683424509324425 ) ) ;
#19084 = DIRECTION ( 'NONE',  ( -1.060575238724910366E-16, 0.4999999999999951705, -0.8660254037844414832 ) ) ;
#19085 = ORIENTED_EDGE ( 'NONE', *, *, #22071, .F. ) ;
#19086 = EDGE_CURVE ( 'NONE', #9804, #6666, #21942, .T. ) ;
#19087 = PRODUCT_DEFINITION_SHAPE ( 'NONE', 'NONE',  #23708 ) ;
#19088 = CARTESIAN_POINT ( 'NONE',  ( -69.90000000218495302, 11.76776695296636888, 13.23223304703362579 ) ) ;
#19089 = VECTOR ( 'NONE', #11113, 1000.000000000000000 ) ;
#19090 = CARTESIAN_POINT ( 'NONE',  ( -5.560781378645573980, 0.000000000000000000, -4.000000000000000000 ) ) ;
#19091 = CIRCLE ( 'NONE', #9172, 11.00000000000000000 ) ;
#19092 = DIRECTION ( 'NONE',  ( -1.000000000000000000, -0.000000000000000000, 0.000000000000000000 ) ) ;
#19093 = CARTESIAN_POINT ( 'NONE',  ( 1.432654583217641386, 3.458734125000000770, 19.37500000136560629 ) ) ;
#19094 = AXIS2_PLACEMENT_3D ( 'NONE', #10316, #17252, #17365 ) ;
#19095 = CARTESIAN_POINT ( 'NONE',  ( 4.999999999999999112, 0.000000000000000000, 0.000000000000000000 ) ) ;
#19096 = CARTESIAN_POINT ( 'NONE',  ( 71.00000000109247367, 12.06698730000000275, 14.14382582708705094 ) ) ;
#19097 = VECTOR ( 'NONE', #23452, 1000.000000000000000 ) ;
#19098 = CARTESIAN_POINT ( 'NONE',  ( -7.229187218286264707E-16, 1.417950490603859619E-15, 10.00000000000000888 ) ) ;
#19099 = CARTESIAN_POINT ( 'NONE',  ( 53.65856816583844591, 7.028187705514647554, 16.31069182806492179 ) ) ;
#19100 = CARTESIAN_POINT ( 'NONE',  ( -3.458734125000000326, 0.000000000000000000, -3.262499998634404541 ) ) ;
#19101 = CARTESIAN_POINT ( 'NONE',  ( -3.458734124999998993, -1.432654583217642497, 12.75000000136560629 ) ) ;
#19102 = CARTESIAN_POINT ( 'NONE',  ( 4.000000000000000000, -2.309401076758514915, -5.000000000000000000 ) ) ;
#19103 = CARTESIAN_POINT ( 'NONE',  ( -69.75000000109245946, 11.46158073645647235, 16.46158073645647235 ) ) ;
#19104 = AXIS2_PLACEMENT_3D ( 'NONE', #14661, #3501, #8789 ) ;
#19105 = DIRECTION ( 'NONE',  ( -7.087422195345011518E-32, -1.000000000000000000, 0.000000000000000000 ) ) ;
#19106 = FACE_OUTER_BOUND ( 'NONE', #12209, .T. ) ;
#19107 = ORIENTED_EDGE ( 'NONE', *, *, #23257, .F. ) ;
#19108 = CARTESIAN_POINT ( 'NONE',  ( -70.89999999999999147, 9.999999999999998224, 17.49999999999999645 ) ) ;
#19110 = AXIS2_PLACEMENT_3D ( 'NONE', #22178, #9646, #12881 ) ;
#19109 = SHAPE_REPRESENTATION_RELATIONSHIP ( 'NONE' , 'NONE' ,  #10226, #23619 ) ;
#19111 = CARTESIAN_POINT ( 'NONE',  ( -4.000000000000000000, -1.656854249492383246, 3.487500002731189319 ) ) ;
#19112 = ORIENTED_EDGE ( 'NONE', *, *, #5127, .T. ) ;
#19113 = EDGE_LOOP ( 'NONE', ( #17908, #12342 ) ) ;
#19114 = LINE ( 'NONE', #15318, #13692 ) ;
#19115 = AXIS2_PLACEMENT_3D ( 'NONE', #1877, #20073, #3673 ) ;
#19116 = CARTESIAN_POINT ( 'NONE',  ( 51.00000000000000711, 12.82842712474617741, 12.17157287525379239 ) ) ;
#19117 = ORIENTED_EDGE ( 'NONE', *, *, #6725, .F. ) ;
#19118 = DIRECTION ( 'NONE',  ( -1.000000000000000000, -7.703719777548943412E-32, 0.000000000000000000 ) ) ;
#19119 = VECTOR ( 'NONE', #8845, 1000.000000000000000 ) ;
#19120 = CARTESIAN_POINT ( 'NONE',  ( 69.20000000109246230, 9.143825827087050939, 12.93301269999999370 ) ) ;
#19121 = VECTOR ( 'NONE', #20411, 1000.000000000000000 ) ;
#19122 = CIRCLE ( 'NONE', #4599, 0.2000000000000005107 ) ;
#19123 = CARTESIAN_POINT ( 'NONE',  ( 68.30000000109247082, 9.143825827087049163, 17.06698729999999742 ) ) ;
#19124 = EDGE_LOOP ( 'NONE', ( #1164, #13687, #8947, #20428, #3292 ) ) ;
#19125 = EDGE_CURVE ( 'NONE', #19131, #3314, #23354, .T. ) ;
#19126 = CARTESIAN_POINT ( 'NONE',  ( 4.000000000000000888, 4.898587196589412829E-16, 14.62500000273119660 ) ) ;
#19127 = CARTESIAN_POINT ( 'NONE',  ( 58.59375000000000711, 11.65685424949236193, 10.99999999999998401 ) ) ;
#19128 = CARTESIAN_POINT ( 'NONE',  ( 1.656854249492384135, -3.999999999999999112, 12.43750000273119838 ) ) ;
#19129 = CARTESIAN_POINT ( 'NONE',  ( 2.445694354108821855, -2.445694354108820079, 17.81250000136560274 ) ) ;
#19130 = PLANE ( 'NONE',  #13632 ) ;
#19131 = VERTEX_POINT ( 'NONE', #12884 ) ;
#19132 = DIRECTION ( 'NONE',  ( -7.087422195345011518E-32, -1.000000000000000000, 0.000000000000000000 ) ) ;
#19133 = CYLINDRICAL_SURFACE ( 'NONE', #3271, 2.500000000000002220 ) ;
#19134 = ADVANCED_FACE ( 'NONE', ( #7606 ), #44, .T. ) ;
#19135 = ORIENTED_EDGE ( 'NONE', *, *, #5989, .T. ) ;
#19136 = AXIS2_PLACEMENT_3D ( 'NONE', #8780, #12853, #12383 ) ;
#19137 = FACE_BOUND ( 'NONE', #20325, .T. ) ;
#19138 = FACE_OUTER_BOUND ( 'NONE', #21640, .T. ) ;
#19139 = LINE ( 'NONE', #10185, #16304 ) ;
#19140 = CIRCLE ( 'NONE', #15738, 6.500000000000000888 ) ;
#19141 = CARTESIAN_POINT ( 'NONE',  ( -71.00000000218494733, 9.999999999999998224, 17.49999999999999645 ) ) ;
#19142 = ORIENTED_EDGE ( 'NONE', *, *, #21216, .T. ) ;
#19143 = CARTESIAN_POINT ( 'NONE',  ( 4.000000000000000000, 1.656854249492381248, 0.8625000000000004885 ) ) ;
#19144 = ORIENTED_EDGE ( 'NONE', *, *, #21763, .F. ) ;
#19145 = CARTESIAN_POINT ( 'NONE',  ( 9.920644283265380691E-16, 4.000000000000000000, 10.75000000000001066 ) ) ;
#19146 = LINE ( 'NONE', #699, #3083 ) ;
#19147 = CARTESIAN_POINT ( 'NONE',  ( 10.97149113033275114, -11.25000000000000355, 5.000000000000079936 ) ) ;
#19148 = DIRECTION ( 'NONE',  ( -1.000000000000000000, -0.000000000000000000, 0.000000000000000000 ) ) ;
#19149 = CARTESIAN_POINT ( 'NONE',  ( 68.45000000109247651, 7.933012699999995476, 14.99999999999999645 ) ) ;
#19150 = ORIENTED_EDGE ( 'NONE', *, *, #2874, .T. ) ;
#19151 = VECTOR ( 'NONE', #1767, 1000.000000000000000 ) ;
#19152 = EDGE_CURVE ( 'NONE', #22180, #13955, #9180, .T. ) ;
#19153 = DIRECTION ( 'NONE',  ( 0.3420201433256622181, 0.9396926207859107594, -6.162975822039141593E-32 ) ) ;
#19154 = EDGE_CURVE ( 'NONE', #14420, #9029, #18725, .T. ) ;
#19155 = FACE_OUTER_BOUND ( 'NONE', #23049, .T. ) ;
#19156 = CARTESIAN_POINT ( 'NONE',  ( 70.55000000109245661, 11.46158073645647235, 16.46158073645647235 ) ) ;
#19157 = CARTESIAN_POINT ( 'NONE',  ( 3.458734125000001214, 4.235727675282971730E-16, 11.93750000136560629 ) ) ;
#19158 = CARTESIAN_POINT ( 'NONE',  ( 0.000000000000000000, 0.000000000000000000, 5.000000000000008882 ) ) ;
#19159 = DIRECTION ( 'NONE',  ( -1.000000000000000000, 0.000000000000000000, 0.000000000000000000 ) ) ;
#19160 = ORIENTED_EDGE ( 'NONE', *, *, #4130, .F. ) ;
#19161 = CARTESIAN_POINT ( 'NONE',  ( -1.656854249492381248, -3.999999999999999112, 1.487500000000001377 ) ) ;
#19162 = CARTESIAN_POINT ( 'NONE',  ( -90.00000000000000000, 8.247996192257451316E-16, 6.735000000000022524 ) ) ;
#19163 = LINE ( 'NONE', #20940, #8944 ) ;
#19164 = CARTESIAN_POINT ( 'NONE',  ( -2.449293598294706907E-16, 4.000000000000000000, -0.9499999999999977351 ) ) ;
#19165 = ADVANCED_FACE ( 'NONE', ( #20140 ), #271, .F. ) ;
#19166 = ADVANCED_FACE ( 'NONE', ( #5913 ), #5671, .T. ) ;
#19167 = ORIENTED_EDGE ( 'NONE', *, *, #21984, .T. ) ;
#19168 = CARTESIAN_POINT ( 'NONE',  ( 14.99999999999995737, -15.00000000000000000, -50.00000000000000000 ) ) ;
#19169 = ORIENTED_EDGE ( 'NONE', *, *, #6631, .T. ) ;
#19170 = CARTESIAN_POINT ( 'NONE',  ( -68.95000000109247651, 11.46158073645647235, 16.46158073645647235 ) ) ;
#19171 = CONTEXT_DEPENDENT_SHAPE_REPRESENTATION ( #11321, #2036 ) ;
#19172 = EDGE_LOOP ( 'NONE', ( #17157, #21759, #15915, #21296 ) ) ;
#19173 = DIRECTION ( 'NONE',  ( -1.000000000000000000, 0.000000000000000000, 0.000000000000000000 ) ) ;
#19174 = EDGE_LOOP ( 'NONE', ( #17627, #22856, #3136, #4110 ) ) ;
#19175 = VECTOR ( 'NONE', #23458, 1000.000000000000000 ) ;
#19176 = ORIENTED_EDGE ( 'NONE', *, *, #877, .F. ) ;
#19177 = CARTESIAN_POINT ( 'NONE',  ( 1.872352939448454495E-15, -3.458734125000000770, 14.93750000136560452 ) ) ;
#19178 = CARTESIAN_POINT ( 'NONE',  ( -7.878064769667250999, -11.25000000000000355, 5.000000000000079936 ) ) ;
#19179 = CARTESIAN_POINT ( 'NONE',  ( 37.82128094071656932, -8.974600000000002353, 5.000000000000079936 ) ) ;
#19180 = EDGE_CURVE ( 'NONE', #2366, #17335, #18244, .T. ) ;
#19181 = CARTESIAN_POINT ( 'NONE',  ( 66.85000000109248219, 9.999999999999998224, 12.93301269999999192 ) ) ;
#19182 = CARTESIAN_POINT ( 'NONE',  ( -67.55000000109247082, 8.538419263543522320, 16.46158073645647235 ) ) ;
#19183 = EDGE_CURVE ( 'NONE', #13486, #2500, #7377, .T. ) ;
#19184 = CARTESIAN_POINT ( 'NONE',  ( -71.39999999999999147, 11.76776695296636888, 13.23223304703362579 ) ) ;
#19185 = CARTESIAN_POINT ( 'NONE',  ( 53.77893183416158251, 8.825410453826341595, 11.97181229448535511 ) ) ;
#19186 = DIRECTION ( 'NONE',  ( 0.000000000000000000, 0.000000000000000000, -1.000000000000000000 ) ) ;
#19187 = CARTESIAN_POINT ( 'NONE',  ( -3.458734125000000770, 1.432654583217640498, 4.925000001365594571 ) ) ;
#19188 = DIRECTION ( 'NONE',  ( -1.000000000000000000, 0.000000000000000000, 0.000000000000000000 ) ) ;
#19189 = CARTESIAN_POINT ( 'NONE',  ( 1.656854249492381470, 4.000000000000000000, 13.81250000273119483 ) ) ;
#19190 = CYLINDRICAL_SURFACE ( 'NONE', #22951, 2.500000000000002220 ) ;
#19191 = EDGE_CURVE ( 'NONE', #9434, #21422, #14685, .T. ) ;
#19192 = EDGE_CURVE ( 'NONE', #13424, #7292, #14637, .T. ) ;
#19193 = VERTEX_POINT ( 'NONE', #2425 ) ;
#19194 = DIRECTION ( 'NONE',  ( -1.000000000000000000, -0.000000000000000000, 0.000000000000000000 ) ) ;
#19195 = ORIENTED_EDGE ( 'NONE', *, *, #903, .T. ) ;
#19196 = CARTESIAN_POINT ( 'NONE',  ( 52.18518183416157541, 10.06805114094562548, 11.99999999999999645 ) ) ;
#19197 = CARTESIAN_POINT ( 'NONE',  ( 6.353591512924457348E-16, -3.458734125000000326, -0.01249999863440348635 ) ) ;
#19198 = CARTESIAN_POINT ( 'NONE',  ( -3.458734125000000326, 1.432654583217640276, 1.675000001365597235 ) ) ;
#19199 = EDGE_LOOP ( 'NONE', ( #21153, #1607, #11904, #17721 ) ) ;
#19200 = CARTESIAN_POINT ( 'NONE',  ( -5.479999999999998650, 6.711064459327494520E-16, 2.039999999999998259 ) ) ;
#19201 = DIRECTION ( 'NONE',  ( -1.000000000000000000, -0.000000000000000000, -0.000000000000000000 ) ) ;
#19202 = VERTEX_POINT ( 'NONE', #6516 ) ;
#19203 = DIRECTION ( 'NONE',  ( -1.000000000000000000, -0.000000000000000000, -0.000000000000000000 ) ) ;
#19204 = EDGE_LOOP ( 'NONE', ( #816, #16508 ) ) ;
#19205 = CARTESIAN_POINT ( 'NONE',  ( 56.75231816583843170, 7.926799079670502124, 17.16943976678978245 ) ) ;
#19206 = CARTESIAN_POINT ( 'NONE',  ( -69.40000000218495302, 9.999999999999998224, 17.49999999999999645 ) ) ;
#19207 = CARTESIAN_POINT ( 'NONE',  ( -72.15000000109247935, 9.999999999999998224, 17.06698730000000097 ) ) ;
#19208 = CARTESIAN_POINT ( 'NONE',  ( -3.999999999999999112, 0.000000000000000000, 15.00000000000001066 ) ) ;
#19209 = CARTESIAN_POINT ( 'NONE',  ( -3.458734124999999437, 1.432654583217640498, 18.62500000136560629 ) ) ;
#19210 = CARTESIAN_POINT ( 'NONE',  ( 4.000000000000000888, 1.656854249492381248, 13.68750000273119483 ) ) ;
#19211 = CARTESIAN_POINT ( 'NONE',  ( -70.89999999999999147, 9.999999999999998224, 17.49999999999999645 ) ) ;
#19212 = CARTESIAN_POINT ( 'NONE',  ( 69.25000000109247367, 9.999999999999998224, 12.93301269999999192 ) ) ;
#19213 = CARTESIAN_POINT ( 'NONE',  ( 45.00000000000000000, -10.00000000000001599, 34.11836509645782201 ) ) ;
#19214 = CARTESIAN_POINT ( 'NONE',  ( 55.90856816583843880, 12.97181229448534978, 13.68930817193506755 ) ) ;
#19215 = CARTESIAN_POINT ( 'NONE',  ( 3.458734125000001214, -1.432654583217639610, 1.425000001365596791 ) ) ;
#19216 = CARTESIAN_POINT ( 'NONE',  ( 3.458734125000001658, 4.235727675282972223E-16, 11.18750000136560452 ) ) ;
#19217 = AXIS2_PLACEMENT_3D ( 'NONE', #11262, #213, #7543 ) ;
#19218 = ADVANCED_FACE ( 'NONE', ( #13589, #15631, #10118, #8089 ), #17411, .F. ) ;
#19219 = DIRECTION ( 'NONE',  ( -0.7071067811865364705, 8.659560562355067211E-17, -0.7071067811865584529 ) ) ;
#19220 = CARTESIAN_POINT ( 'NONE',  ( -69.10000000109246798, 9.143825827087049163, 17.06698730000000097 ) ) ;
#19221 = ADVANCED_FACE ( 'NONE', ( #8308 ), #862, .T. ) ;
#19222 = DIRECTION ( 'NONE',  ( 0.000000000000000000, 0.8090169943749487835, -0.5877852522924714718 ) ) ;
#19223 = CYLINDRICAL_SURFACE ( 'NONE', #18921, 2.500000000000000444 ) ;
#19224 = ORIENTED_EDGE ( 'NONE', *, *, #21666, .T. ) ;
#19225 = CARTESIAN_POINT ( 'NONE',  ( 4.000000000000000000, -2.309401076758516691, -0.4999999999999995559 ) ) ;
#19226 = ORIENTED_EDGE ( 'NONE', *, *, #14664, .T. ) ;
#19227 = ORIENTED_EDGE ( 'NONE', *, *, #23437, .F. ) ;
#19228 = DIRECTION ( 'NONE',  ( -1.000000000000000000, -0.000000000000000000, -0.000000000000000000 ) ) ;
#19229 = CARTESIAN_POINT ( 'NONE',  ( -66.59999999999999432, 11.76776695296636888, 13.23223304703362579 ) ) ;
#19230 = ORIENTED_EDGE ( 'NONE', *, *, #15865, .T. ) ;
#19231 = CARTESIAN_POINT ( 'NONE',  ( 27.50000000000000000, 7.500000000000001776, -33.66025403784446723 ) ) ;
#19232 = CARTESIAN_POINT ( 'NONE',  ( 68.05000000109247082, 9.999999999999998224, 17.06698730000000097 ) ) ;
#19233 = CARTESIAN_POINT ( 'NONE',  ( 66.90000000109246514, 7.933012699999995476, 14.14382582708705094 ) ) ;
#19234 = AXIS2_PLACEMENT_3D ( 'NONE', #15993, #14322, #12769 ) ;
#19235 = VERTEX_POINT ( 'NONE', #11804 ) ;
#19236 = FACE_BOUND ( 'NONE', #733, .T. ) ;
#19237 = CARTESIAN_POINT ( 'NONE',  ( 53.90625000000000000, 13.99999999999999289, 13.34314575050759544 ) ) ;
#19238 = CARTESIAN_POINT ( 'NONE',  ( 118.3095189484530181, 14.69846310392956745, 35.82846581308617573 ) ) ;
#19239 = CARTESIAN_POINT ( 'NONE',  ( 1.025207404391860050E-15, 3.458734125000000326, 19.18750000136560629 ) ) ;
#19240 = CARTESIAN_POINT ( 'NONE',  ( 4.999999999999999112, -9.915734732513184824, -4.762163868918378284 ) ) ;
#19241 = FACE_OUTER_BOUND ( 'NONE', #5676, .T. ) ;
#19242 = ORIENTED_EDGE ( 'NONE', *, *, #23031, .T. ) ;
#19243 = DIRECTION ( 'NONE',  ( 0.000000000000000000, 0.000000000000000000, -1.000000000000000000 ) ) ;
#19244 = DIRECTION ( 'NONE',  ( -1.000000000000000000, -0.000000000000000000, -0.000000000000000000 ) ) ;
#19245 = PLANE ( 'NONE',  #12361 ) ;
#19246 = VERTEX_POINT ( 'NONE', #15278 ) ;
#19247 = CIRCLE ( 'NONE', #22298, 6.735000000000022524 ) ;
#19248 = CARTESIAN_POINT ( 'NONE',  ( 1.393927851585479161, -4.043713361053543842, -3.526374918436840922 ) ) ;
#19249 = CARTESIAN_POINT ( 'NONE',  ( 2.828427124746192067, -2.828427124746189847, 11.50000000273119660 ) ) ;
#19251 = AXIS2_PLACEMENT_3D ( 'NONE', #7431, #11028, #21774 ) ;
#19250 = PRODUCT_RELATED_PRODUCT_CATEGORY ( 'part', '', ( #11846 ) ) ;
#19252 = CARTESIAN_POINT ( 'NONE',  ( 71.25000000218494733, 7.499999999999996447, 13.96446609406725514 ) ) ;
#19253 = ORIENTED_EDGE ( 'NONE', *, *, #4470, .T. ) ;
#19254 = CARTESIAN_POINT ( 'NONE',  ( -68.25000000218493312, 11.03553390593269157, 12.49999999999994849 ) ) ;
#19255 = ORIENTED_EDGE ( 'NONE', *, *, #18037, .F. ) ;
#19256 = EDGE_CURVE ( 'NONE', #22731, #375, #17174, .T. ) ;
#19257 = DIRECTION ( 'NONE',  ( 1.000000000000000000, -0.000000000000000000, -0.000000000000000000 ) ) ;
#19258 = CARTESIAN_POINT ( 'NONE',  ( 70.60000000218494165, 9.999999999999998224, 12.49999999999999289 ) ) ;
#19259 = CARTESIAN_POINT ( 'NONE',  ( -2.828427124746188515, -2.828427124746190735, 16.12500000000001066 ) ) ;
#19260 = CARTESIAN_POINT ( 'NONE',  ( -2.000000000000002665, -3.464101615137770374, -3.142992957459237680 ) ) ;
#19261 = CARTESIAN_POINT ( 'NONE',  ( 67.90000000109246514, 10.85617417291294551, 12.93301269999999192 ) ) ;
#19262 = ORIENTED_EDGE ( 'NONE', *, *, #13788, .T. ) ;
#19263 = DIRECTION ( 'NONE',  ( -1.224646799147353207E-16, 0.000000000000000000, -1.000000000000000000 ) ) ;
#19264 = CARTESIAN_POINT ( 'NONE',  ( -3.999999999999998224, -1.656854249492383024, 10.18750000273119660 ) ) ;
#19265 = CARTESIAN_POINT ( 'NONE',  ( 69.55000000109247082, 11.46158073645647235, 13.53841926354352232 ) ) ;
#19266 = CARTESIAN_POINT ( 'NONE',  ( 3.458734125000001658, 1.432654583217640498, 17.25000000136560629 ) ) ;
#19267 = LINE ( 'NONE', #1289, #6320 ) ;
#19268 = CARTESIAN_POINT ( 'NONE',  ( 4.999999999999999112, -1.464956435139466828, -10.90201369670500320 ) ) ;
#19269 = ORIENTED_EDGE ( 'NONE', *, *, #10383, .F. ) ;
#19270 = CARTESIAN_POINT ( 'NONE',  ( 4.000000000000000000, 4.898587196589412829E-16, -1.199999999999997957 ) ) ;
#19271 = CARTESIAN_POINT ( 'NONE',  ( -18.73663160323380339, -9.000000000000003553, 5.000000000000079936 ) ) ;
#19272 = CARTESIAN_POINT ( 'NONE',  ( 4.000000000000000000, 0.000000000000000000, 19.04999999999996874 ) ) ;
#19273 = LINE ( 'NONE', #17499, #17579 ) ;
#19274 = ORIENTED_EDGE ( 'NONE', *, *, #14442, .T. ) ;
#19275 = FACE_OUTER_BOUND ( 'NONE', #19721, .T. ) ;
#19276 = ORIENTED_EDGE ( 'NONE', *, *, #91, .T. ) ;
#19277 = CARTESIAN_POINT ( 'NONE',  ( -66.30000000109247082, 10.85617417291294551, 12.93301269999999370 ) ) ;
#19278 = ORIENTED_EDGE ( 'NONE', *, *, #3597, .T. ) ;
#19279 = CARTESIAN_POINT ( 'NONE',  ( -4.000000000000000888, 1.656854249492380582, -1.637499997268811569 ) ) ;
#19280 = ORIENTED_EDGE ( 'NONE', *, *, #14986, .T. ) ;
#19281 = ADVANCED_FACE ( 'NONE', ( #20741 ), #9756, .T. ) ;
#19282 = ADVANCED_FACE ( 'NONE', ( #22662 ), #6272, .F. ) ;
#19283 = EDGE_LOOP ( 'NONE', ( #19520, #19678 ) ) ;
#19284 = CARTESIAN_POINT ( 'NONE',  ( 1.432654583217643163, -3.458734124999999882, 14.00000000136560629 ) ) ;
#19285 = CARTESIAN_POINT ( 'NONE',  ( 6.500000000000000000, 3.752776749732573247, -3.119443416399232394 ) ) ;
#19286 = CARTESIAN_POINT ( 'NONE',  ( -66.00000000109247367, 9.143825827087050939, 12.93301269999999370 ) ) ;
#19287 = CARTESIAN_POINT ( 'NONE',  ( 35.00000000000000000, 1.500000000000009992, -17.32050807568893092 ) ) ;
#19288 = EDGE_CURVE ( 'NONE', #15638, #22615, #8197, .T. ) ;
#19289 = CARTESIAN_POINT ( 'NONE',  ( -71.64999999999997726, 11.03553390593273598, 17.50000000000000355 ) ) ;
#19290 = AXIS2_PLACEMENT_3D ( 'NONE', #5879, #13203, #2392 ) ;
#19291 = CARTESIAN_POINT ( 'NONE',  ( -1.600000000000004086, 0.000000000000000000, -8.265000000000021885 ) ) ;
#19292 = CARTESIAN_POINT ( 'NONE',  ( 59.59143183416158962, 11.72490539043799984, 11.02818770551463246 ) ) ;
#19293 = PLANE ( 'NONE',  #117 ) ;
#19294 = CARTESIAN_POINT ( 'NONE',  ( -3.458734125000000326, -1.432654583217642497, 0.05000000136559582670 ) ) ;
#19295 = CARTESIAN_POINT ( 'NONE',  ( 67.25000000218494733, 7.499999999999996447, 13.96446609406725514 ) ) ;
#19296 = DIRECTION ( 'NONE',  ( 0.000000000000000000, 1.000000000000000000, -1.224646799147353207E-16 ) ) ;
#19297 = CARTESIAN_POINT ( 'NONE',  ( 1.971781867644420635E-15, -4.000000000000000000, 12.37500000273119838 ) ) ;
#19298 = CARTESIAN_POINT ( 'NONE',  ( 4.999999999999999112, 2.223716399045689407, -8.461683424509292450 ) ) ;
#19299 = VERTEX_POINT ( 'NONE', #4347 ) ;
#19300 = DIRECTION ( 'NONE',  ( 0.9396926207859107594, -0.3420201433256623291, 3.697785493223492838E-32 ) ) ;
#19301 = ORIENTED_EDGE ( 'NONE', *, *, #13970, .F. ) ;
#19302 = CARTESIAN_POINT ( 'NONE',  ( 55.27893183416158251, 8.825410453826341595, 11.97181229448535511 ) ) ;
#19303 = SURFACE_STYLE_USAGE ( .BOTH. , #17300 ) ;
#19304 = CARTESIAN_POINT ( 'NONE',  ( -2.117863837641485618E-16, 3.458734125000000326, 0.4875000013655952369 ) ) ;
#19305 = ORIENTED_EDGE ( 'NONE', *, *, #7667, .F. ) ;
#19306 = CARTESIAN_POINT ( 'NONE',  ( 0.000000000000000000, 0.000000000000000000, 0.000000000000000000 ) ) ;
#19307 = VECTOR ( 'NONE', #13298, 1000.000000000000000 ) ;
#19308 = EDGE_CURVE ( 'NONE', #17335, #2869, #15158, .T. ) ;
#19309 = ORIENTED_EDGE ( 'NONE', *, *, #3478, .F. ) ;
#19310 = VECTOR ( 'NONE', #11257, 999.9999999999998863 ) ;
#19311 = DIRECTION ( 'NONE',  ( -0.3373062947069096484, 0.9413949561959079615, 0.000000000000000000 ) ) ;
#19312 = ORIENTED_EDGE ( 'NONE', *, *, #19903, .T. ) ;
#19313 = CARTESIAN_POINT ( 'NONE',  ( 58.06481816583843170, 6.999999999999998224, 15.06805114094563436 ) ) ;
#19314 = CARTESIAN_POINT ( 'NONE',  ( -67.10000000218495586, 8.232233047033627571, 16.76776695296636532 ) ) ;
#19315 = EDGE_CURVE ( 'NONE', #13219, #19809, #17068, .T. ) ;
#19316 = LINE ( 'NONE', #19090, #14457 ) ;
#19317 = EDGE_CURVE ( 'NONE', #1746, #22551, #553, .T. ) ;
#19318 = DIRECTION ( 'NONE',  ( 0.000000000000000000, 0.000000000000000000, -1.000000000000000000 ) ) ;
#19319 = CARTESIAN_POINT ( 'NONE',  ( -2.445694354108819191, 2.445694354108820523, 18.56250000136560629 ) ) ;
#19320 = CARTESIAN_POINT ( 'NONE',  ( 2.828427124746192067, -2.828427124746189847, 15.50000000273119660 ) ) ;
#19321 = CARTESIAN_POINT ( 'NONE',  ( 57.84375000000000711, 8.757359312880723223, 18.00000000000000355 ) ) ;
#19322 = CARTESIAN_POINT ( 'NONE',  ( 68.85000000109248219, 9.999999999999998224, 17.06698730000000097 ) ) ;
#19324 = CARTESIAN_POINT ( 'NONE',  ( 68.20000000218495018, 9.999999999999998224, 12.49999999999999289 ) ) ;
#19323 = CIRCLE ( 'NONE', #11726, 4.000000000000002665 ) ;
#19325 = CARTESIAN_POINT ( 'NONE',  ( 57.84375000000000711, 8.757359312880723223, 18.00000000000000355 ) ) ;
#19326 = AXIS2_PLACEMENT_3D ( 'NONE', #17234, #6208, #4641 ) ;
#19327 = CARTESIAN_POINT ( 'NONE',  ( 6.353591512924457348E-16, -3.458734125000000770, 1.237500001365595903 ) ) ;
#19328 = CYLINDRICAL_SURFACE ( 'NONE', #16192, 11.00000000000000000 ) ;
#19329 = LINE ( 'NONE', #10267, #22559 ) ;
#19330 = CARTESIAN_POINT ( 'NONE',  ( -68.75000000109245946, 11.46158073645647235, 13.53841926354352232 ) ) ;
#19331 = VERTEX_POINT ( 'NONE', #18840 ) ;
#19332 = CARTESIAN_POINT ( 'NONE',  ( 4.999999999999999112, -7.360373001730951437, 4.729683950898845524 ) ) ;
#19333 = DIRECTION ( 'NONE',  ( 0.000000000000000000, 0.000000000000000000, 1.000000000000000000 ) ) ;
#19334 = ORIENTED_EDGE ( 'NONE', *, *, #2197, .F. ) ;
#19335 = CARTESIAN_POINT ( 'NONE',  ( -1.656854249492380138, -3.999999999999999112, 15.31250000273119660 ) ) ;
#19336 = CARTESIAN_POINT ( 'NONE',  ( -4.000000000000000888, 1.656854249492380804, -0.6374999972688125682 ) ) ;
#19337 = ORIENTED_EDGE ( 'NONE', *, *, #112, .F. ) ;
#19338 = CIRCLE ( 'NONE', #14397, 11.00000000000000000 ) ;
#19339 = ORIENTED_EDGE ( 'NONE', *, *, #18595, .F. ) ;
#19340 = DIRECTION ( 'NONE',  ( -0.3420201433256622181, 0.9396926207859106484, 1.232595164407828100E-31 ) ) ;
#19341 = DIRECTION ( 'NONE',  ( 0.000000000000000000, 0.000000000000000000, 1.000000000000000000 ) ) ;
#19342 = ORIENTED_EDGE ( 'NONE', *, *, #14972, .T. ) ;
#19343 = CARTESIAN_POINT ( 'NONE',  ( 1.236993788156008760E-15, 0.000000000000000000, 21.31370849898476649 ) ) ;
#19344 = ADVANCED_FACE ( 'NONE', ( #628 ), #6157, .F. ) ;
#19345 = CARTESIAN_POINT ( 'NONE',  ( 68.25000000109247367, 7.933012699999995476, 14.99999999999999645 ) ) ;
#19346 = EDGE_CURVE ( 'NONE', #9768, #21282, #8832, .T. ) ;
#19347 = CARTESIAN_POINT ( 'NONE',  ( 68.10000000109245377, 12.06698730000000275, 15.85617417291294196 ) ) ;
#19348 = CYLINDRICAL_SURFACE ( 'NONE', #13545, 4.000000000000001776 ) ;
#19349 = DIRECTION ( 'NONE',  ( -1.000000000000000000, -0.000000000000000000, 0.000000000000000000 ) ) ;
#19350 =( BOUNDED_CURVE ( )  B_SPLINE_CURVE ( 2, ( #15726, #22996, #6602, #13920, #21175, #19388, #17628, #21289, #4912 ),
 .UNSPECIFIED., .F., .F. ) 
 B_SPLINE_CURVE_WITH_KNOTS ( ( 3, 2, 2, 2, 3 ),
 ( 0.5500000000000000444, 0.5625000000000000000, 0.5749999999999999556, 0.5875000000000000222, 0.5999999999999999778 ),
 .UNSPECIFIED. ) 
 CURVE ( )  GEOMETRIC_REPRESENTATION_ITEM ( )  RATIONAL_B_SPLINE_CURVE ( ( 1.000000000000000000, 0.9238795325112867385, 1.000000000000000000, 0.9238795325112867385, 1.000000000000000000, 0.9238795325112867385, 1.000000000000000000, 0.9238795325112867385, 1.000000000000000000 ) ) 
 REPRESENTATION_ITEM ( '' )  );
#19351 = CARTESIAN_POINT ( 'NONE',  ( 56.71875000000000711, 14.00000000000000888, 16.65685424949235482 ) ) ;
#19352 = CARTESIAN_POINT ( 'NONE',  ( -3.458734125000000326, 0.000000000000000000, 4.737500001365595459 ) ) ;
#19353 = CARTESIAN_POINT ( 'NONE',  ( -2.445694354108819191, 2.445694354108820523, 13.31250000136560452 ) ) ;
#19354 = LINE ( 'NONE', #1151, #14372 ) ;
#19355 = FACE_OUTER_BOUND ( 'NONE', #18611, .T. ) ;
#19356 = ORIENTED_EDGE ( 'NONE', *, *, #13918, .T. ) ;
#19357 = DIRECTION ( 'NONE',  ( -1.000000000000000000, -0.000000000000000000, 0.000000000000000000 ) ) ;
#19358 = CARTESIAN_POINT ( 'NONE',  ( -4.000000000000000000, 1.285413958923598443, -3.623488494345327382 ) ) ;
#19359 = DIRECTION ( 'NONE',  ( -1.000000000000000000, 0.000000000000000000, 0.000000000000000000 ) ) ;
#19360 = VERTEX_POINT ( 'NONE', #17874 ) ;
#19361 = CARTESIAN_POINT ( 'NONE',  ( -6.473970235329672780E-16, -4.862606272033106691, -3.745885042887442395 ) ) ;
#19362 = CARTESIAN_POINT ( 'NONE',  ( 71.55000000109247082, 8.538419263543524096, 13.53841926354352054 ) ) ;
#19363 = ORIENTED_EDGE ( 'NONE', *, *, #7038, .F. ) ;
#19364 = CARTESIAN_POINT ( 'NONE',  ( -68.20000000218495018, 9.999999999999998224, 12.49999999999999289 ) ) ;
#19365 = VERTEX_POINT ( 'NONE', #10363 ) ;
#19366 = DIRECTION ( 'NONE',  ( 0.000000000000000000, -1.000000000000000000, 0.000000000000000000 ) ) ;
#19367 = ADVANCED_FACE ( 'NONE', ( #14297 ), #12387, .F. ) ;
#19368 = CARTESIAN_POINT ( 'NONE',  ( 71.70000000218495018, 11.76776695296636888, 16.76776695296636532 ) ) ;
#19369 = VECTOR ( 'NONE', #16344, 1000.000000000000000 ) ;
#19370 = CARTESIAN_POINT ( 'NONE',  ( 1.971781867644420635E-15, -4.000000000000000000, 19.25000000000001066 ) ) ;
#19371 = CARTESIAN_POINT ( 'NONE',  ( 2.828427124746191179, 2.828427124746190291, 11.62500000000001066 ) ) ;
#19372 = CARTESIAN_POINT ( 'NONE',  ( 67.95000000109247651, 11.46158073645647235, 13.53841926354352232 ) ) ;
#19373 = ORIENTED_EDGE ( 'NONE', *, *, #18231, .T. ) ;
#19374 = LINE ( 'NONE', #20931, #19841 ) ;
#19375 = DIRECTION ( 'NONE',  ( -1.000000000000000000, -0.000000000000000000, -0.000000000000000000 ) ) ;
#19376 = CARTESIAN_POINT ( 'NONE',  ( 69.50000000109247367, 10.85617417291294551, 12.93301269999999370 ) ) ;
#19377 = CARTESIAN_POINT ( 'NONE',  ( -1.432654583217639166, 3.458734125000000770, 19.50000000136560629 ) ) ;
#19378 = CARTESIAN_POINT ( 'NONE',  ( 0.000000000000000000, 0.000000000000000000, -3.700000000000000178 ) ) ;
#19379 = CIRCLE ( 'NONE', #2555, 2.500000000000000444 ) ;
#19380 = DIRECTION ( 'NONE',  ( -1.000000000000000000, 0.000000000000000000, 0.000000000000000000 ) ) ;
#19381 = VERTEX_POINT ( 'NONE', #3135 ) ;
#19382 = CARTESIAN_POINT ( 'NONE',  ( 4.000000000000000000, 4.898587196589412829E-16, -2.199999999999998845 ) ) ;
#19383 = CARTESIAN_POINT ( 'NONE',  ( 2.828427124746191179, 2.828427124746190291, 15.62500000000001066 ) ) ;
#19384 = DIRECTION ( 'NONE',  ( 0.000000000000000000, 0.000000000000000000, 1.000000000000000000 ) ) ;
#19385 = DIRECTION ( 'NONE',  ( -0.9413949561959078505, -0.3373062947069098150, 1.152876319838781169E-16 ) ) ;
#19386 =( BOUNDED_CURVE ( )  B_SPLINE_CURVE ( 2, ( #333, #2696, #4489, #17205, #6301, #1125, #14990, #20880, #10038 ),
 .UNSPECIFIED., .F., .F. ) 
 B_SPLINE_CURVE_WITH_KNOTS ( ( 3, 2, 2, 2, 3 ),
 ( 0.2500000000000006661, 0.2656250000000005551, 0.2812500000000004441, 0.2968750000000003886, 0.3125000000000002776 ),
 .UNSPECIFIED. ) 
 CURVE ( )  GEOMETRIC_REPRESENTATION_ITEM ( )  RATIONAL_B_SPLINE_CURVE ( ( 0.9999999999999967804, 0.9238795325112899581, 1.000000000000000000, 0.9238795325112867385, 1.000000000000000000, 0.9238795325112867385, 1.000000000000000000, 0.9238795325112854062, 1.000000000000001332 ) ) 
 REPRESENTATION_ITEM ( '' )  );
#19387 = ORIENTED_EDGE ( 'NONE', *, *, #1108, .F. ) ;
#19388 = CARTESIAN_POINT ( 'NONE',  ( -1.656854249492380138, -3.999999999999999112, 13.31250000273119660 ) ) ;
#19389 = VERTEX_POINT ( 'NONE', #6626 ) ;
#19390 = AXIS2_PLACEMENT_3D ( 'NONE', #14079, #5191, #1349 ) ;
#19391 = CARTESIAN_POINT ( 'NONE',  ( -67.50000000109245946, 9.143825827087049163, 17.06698729999999742 ) ) ;
#19392 = ITEM_DEFINED_TRANSFORMATION ( 'NONE', 'NONE', #1875,  #7318 ) ;
#19393 = VERTEX_POINT ( 'NONE', #23489 ) ;
#19394 = DIRECTION ( 'NONE',  ( 0.000000000000000000, -1.000000000000000000, 0.000000000000000000 ) ) ;
#19395 = ORIENTED_EDGE ( 'NONE', *, *, #23128, .T. ) ;
#19396 =( REPRESENTATION_RELATIONSHIP ('NONE','NONE', #8403, #18175 ) REPRESENTATION_RELATIONSHIP_WITH_TRANSFORMATION ( #16918 )SHAPE_REPRESENTATION_RELATIONSHIP( ) );
#19397 = ORIENTED_EDGE ( 'NONE', *, *, #16884, .T. ) ;
#19398 = CARTESIAN_POINT ( 'NONE',  ( 1.432654583217641386, 3.458734125000000770, 11.37500000136560452 ) ) ;
#19399 = DIRECTION ( 'NONE',  ( 0.3420201433256622181, 0.9396926207859107594, -6.162975822039141593E-32 ) ) ;
#19400 = AXIS2_PLACEMENT_3D ( 'NONE', #22126, #14304, #7548 ) ;
#19401 = CARTESIAN_POINT ( 'NONE',  ( -66.05000000109247082, 9.999999999999998224, 12.93301269999999192 ) ) ;
#19402 = CARTESIAN_POINT ( 'NONE',  ( 6.396109596766202721, -9.000000000000003553, 5.000000000000079936 ) ) ;
#19403 = CARTESIAN_POINT ( 'NONE',  ( -71.39999999999999147, 11.76776695296636888, 13.23223304703362579 ) ) ;
#19404 = LINE ( 'NONE', #3487, #22503 ) ;
#19405 = CARTESIAN_POINT ( 'NONE',  ( 59.99999999999996447, 10.90022099756737717, 18.35387496708138499 ) ) ;
#19406 = AXIS2_PLACEMENT_3D ( 'NONE', #10078, #17366, #4422 ) ;
#19407 = EDGE_CURVE ( 'NONE', #17227, #19630, #4938, .T. ) ;
#19408 = CARTESIAN_POINT ( 'NONE',  ( 2.445694354108820967, -2.445694354108820079, 1.362500001365595903 ) ) ;
#19409 = CARTESIAN_POINT ( 'NONE',  ( 4.999999999999999112, 0.000000000000000000, 0.000000000000000000 ) ) ;
#19410 = DIRECTION ( 'NONE',  ( 0.000000000000000000, -0.8090169943749532244, 0.5877852522924653655 ) ) ;
#19411 = CARTESIAN_POINT ( 'NONE',  ( -2.828427124746189403, 2.828427124746190291, 12.00000000273119660 ) ) ;
#19412 = DIRECTION ( 'NONE',  ( 0.3420201433256622181, -0.9396926207859107594, 0.000000000000000000 ) ) ;
#19413 = AXIS2_PLACEMENT_3D ( 'NONE', #5449, #9190, #14583 ) ;
#19414 = VERTEX_POINT ( 'NONE', #3011 ) ;
#19415 = VECTOR ( 'NONE', #10246, 1000.000000000000000 ) ;
#19416 = ORIENTED_EDGE ( 'NONE', *, *, #147, .F. ) ;
#19417 = CARTESIAN_POINT ( 'NONE',  ( 59.96643183416158251, 6.028187705514633343, 13.27509460956200016 ) ) ;
#19418 = CARTESIAN_POINT ( 'NONE',  ( -70.15000000109247935, 11.46158073645647235, 13.53841926354352232 ) ) ;
#19419 = CARTESIAN_POINT ( 'NONE',  ( 0.000000000000000000, 0.000000000000000000, 0.000000000000000000 ) ) ;
#19420 = EDGE_CURVE ( 'NONE', #16157, #13512, #9444, .T. ) ;
#19421 = CARTESIAN_POINT ( 'NONE',  ( 0.000000000000000000, -6.478011392632841314, -6.807171995660652897 ) ) ;
#19422 = EDGE_LOOP ( 'NONE', ( #22446, #14663, #3566, #19262, #14182 ) ) ;
#19423 = DIRECTION ( 'NONE',  ( -1.000000000000000000, 0.000000000000000000, 0.000000000000000000 ) ) ;
#19424 = AXIS2_PLACEMENT_3D ( 'NONE', #3737, #5662, #11201 ) ;
#19425 = ORIENTED_EDGE ( 'NONE', *, *, #18561, .T. ) ;
#19426 = CARTESIAN_POINT ( 'NONE',  ( 0.000000000000000000, -9.314797388894882957, -1.239665997526988139 ) ) ;
#19427 = VERTEX_POINT ( 'NONE', #1326 ) ;
#19428 = CARTESIAN_POINT ( 'NONE',  ( 55.62731816583843170, 12.16943976678978601, 17.07320092032949432 ) ) ;
#19429 = MECHANICAL_DESIGN_GEOMETRIC_PRESENTATION_REPRESENTATION (  '', ( #2212 ), #22489 ) ;
#19430 = CARTESIAN_POINT ( 'NONE',  ( -66.00000000218494733, 12.50000000000000000, 14.99999999999999645 ) ) ;
#19431 = DIRECTION ( 'NONE',  ( 0.000000000000000000, 0.000000000000000000, 1.000000000000000000 ) ) ;
#19432 = B_SPLINE_CURVE_WITH_KNOTS ( 'NONE', 3,
 ( #5842, #7424, #14734, #12716, #21993, #5607, #19968, #451 ),
 .UNSPECIFIED., .F., .F.,
 ( 4, 2, 2, 4 ),
 ( 0.003797433802554436334, 0.004743183970586237024, 0.005688934138618036845, 0.007580434474681636489 ),
 .UNSPECIFIED. ) ;
#19433 = VECTOR ( 'NONE', #8023, 1000.000000000000114 ) ;
#19434 = CARTESIAN_POINT ( 'NONE',  ( -71.60000000109246798, 7.933012699999995476, 15.85617417291294196 ) ) ;
#19435 = AXIS2_PLACEMENT_3D ( 'NONE', #4465, #19077, #10012 ) ;
#19436 = CARTESIAN_POINT ( 'NONE',  ( 3.458734125000001658, 4.235727675282972223E-16, 16.18750000136560629 ) ) ;
#19437 = CARTESIAN_POINT ( 'NONE',  ( 4.000000000000000888, 1.656854249492381248, 12.68750000273119660 ) ) ;
#19438 = DIRECTION ( 'NONE',  ( 0.000000000000000000, -0.3090169943749548342, 0.9510565162951509777 ) ) ;
#19439 = FACE_OUTER_BOUND ( 'NONE', #4069, .T. ) ;
#19440 = EDGE_CURVE ( 'NONE', #12636, #8828, #23247, .T. ) ;
#19441 = DIRECTION ( 'NONE',  ( 0.9021819276640002938, 0.000000000000000000, -0.4313557341643536880 ) ) ;
#19442 = CARTESIAN_POINT ( 'NONE',  ( 50.09606816583843880, 11.17458954617364242, 11.97181229448534800 ) ) ;
#19443 = EDGE_CURVE ( 'NONE', #375, #20062, #21441, .T. ) ;
#19444 = CARTESIAN_POINT ( 'NONE',  ( 2.445694354108820967, -2.445694354108820079, 2.362500001365596791 ) ) ;
#19445 = CARTESIAN_POINT ( 'NONE',  ( 67.45000000218493597, 11.03553390593273420, 12.49999999999998934 ) ) ;
#19446 = VECTOR ( 'NONE', #6732, 1000.000000000000000 ) ;
#19447 = PRESENTATION_STYLE_ASSIGNMENT (( #15880 ) ) ;
#19448 = CARTESIAN_POINT ( 'NONE',  ( -67.80000000109247082, 9.143825827087052716, 12.93301269999999192 ) ) ;
#19449 = CIRCLE ( 'NONE', #20958, 0.2000000000000005107 ) ;
#19450 = VERTEX_POINT ( 'NONE', #15751 ) ;
#19451 = LINE ( 'NONE', #7130, #6006 ) ;
#19452 = DIRECTION ( 'NONE',  ( -1.000000000000000000, 0.000000000000000000, 0.000000000000000000 ) ) ;
#19453 = ORIENTED_EDGE ( 'NONE', *, *, #4692, .T. ) ;
#19454 = CARTESIAN_POINT ( 'NONE',  ( 9.537702246766199821, -9.000000000000005329, 10.00000000000008882 ) ) ;
#19455 =( LENGTH_UNIT ( ) NAMED_UNIT ( * ) SI_UNIT ( .MILLI., .METRE. ) );
#19456 = CARTESIAN_POINT ( 'NONE',  ( 4.000000000000000000, 1.656854249492381248, -1.012499997268812901 ) ) ;
#19457 = EDGE_CURVE ( 'NONE', #17245, #5464, #3898, .T. ) ;
#19458 = VERTEX_POINT ( 'NONE', #11775 ) ;
#19459 = EDGE_CURVE ( 'NONE', #17446, #4526, #7077, .T. ) ;
#19460 = ORIENTED_EDGE ( 'NONE', *, *, #23224, .T. ) ;
#19461 = FACE_OUTER_BOUND ( 'NONE', #8548, .T. ) ;
#19462 = VECTOR ( 'NONE', #4653, 1000.000000000000000 ) ;
#19463 = CARTESIAN_POINT ( 'NONE',  ( 4.999999999999999112, 7.360373001730986964, -4.729683950898791345 ) ) ;
#19464 = ORIENTED_EDGE ( 'NONE', *, *, #4733, .T. ) ;
#19465 = CARTESIAN_POINT ( 'NONE',  ( 0.6810597143197052450, 4.461075778259290914, -3.598441714920602053 ) ) ;
#19466 = CARTESIAN_POINT ( 'NONE',  ( 1.656854249492381470, 4.000000000000000000, 11.68750000000001066 ) ) ;
#19467 = AXIS2_PLACEMENT_3D ( 'NONE', #359, #232, #2026 ) ;
#19468 = CARTESIAN_POINT ( 'NONE',  ( -4.000000000000000000, 0.000000000000000000, 1.425000002731187765 ) ) ;
#19469 = VECTOR ( 'NONE', #18301, 1000.000000000000000 ) ;
#19470 = CARTESIAN_POINT ( 'NONE',  ( 68.00000000109245946, 12.06698730000000275, 14.14382582708705094 ) ) ;
#19471 = DIRECTION ( 'NONE',  ( 0.000000000000000000, 0.000000000000000000, 1.000000000000000000 ) ) ;
#19472 = CYLINDRICAL_SURFACE ( 'NONE', #11495, 4.000000000000001776 ) ;
#19473 = AXIS2_PLACEMENT_3D ( 'NONE', #4149, #20782, #4386 ) ;
#19474 = CARTESIAN_POINT ( 'NONE',  ( 57.12731816583843170, 12.87654654797634102, 17.78030770151602979 ) ) ;
#19475 = EDGE_CURVE ( 'NONE', #13926, #17599, #7928, .T. ) ;
#19476 = CARTESIAN_POINT ( 'NONE',  ( -2.445694354108819635, -2.445694354108820523, 4.862500001365595459 ) ) ;
#19477 = CARTESIAN_POINT ( 'NONE',  ( 1.872352939448454495E-15, -3.458734125000000326, 16.68750000136560629 ) ) ;
#19478 = CARTESIAN_POINT ( 'NONE',  ( -9.302608809283439584, -8.974600000000002353, 5.000000000000079936 ) ) ;
#19479 = CYLINDRICAL_SURFACE ( 'NONE', #14726, 4.000000000000001776 ) ;
#19480 = ORIENTED_EDGE ( 'NONE', *, *, #9232, .T. ) ;
#19481 = CARTESIAN_POINT ( 'NONE',  ( -3.553888437116970778, 0.5218273788507123978, 2.039999999999990266 ) ) ;
#19482 = CARTESIAN_POINT ( 'NONE',  ( 4.999999999999999112, -9.241976615262146311, -1.699438267350473097 ) ) ;
#19483 = CARTESIAN_POINT ( 'NONE',  ( -1.656854249492381248, -3.999999999999999112, -1.512499999999997735 ) ) ;
#19484 = EDGE_CURVE ( 'NONE', #18054, #19575, #22755, .T. ) ;
#19485 = VERTEX_POINT ( 'NONE', #19045 ) ;
#19486 = CIRCLE ( 'NONE', #3811, 4.000000000000001776 ) ;
#19487 = DIRECTION ( 'NONE',  ( 0.000000000000000000, 0.000000000000000000, 1.000000000000000000 ) ) ;
#19488 = CARTESIAN_POINT ( 'NONE',  ( -67.45000000000000284, 12.50000000000000000, 13.96446609406725692 ) ) ;
#19489 = CARTESIAN_POINT ( 'NONE',  ( 59.90625000000000711, 13.99999999999999289, 13.34314575050759544 ) ) ;
#19490 = ORIENTED_EDGE ( 'NONE', *, *, #11134, .F. ) ;
#19491 = CARTESIAN_POINT ( 'NONE',  ( 4.999999999999999112, 0.000000000000000000, 0.000000000000000000 ) ) ;
#19492 = VERTEX_POINT ( 'NONE', #6367 ) ;
#19493 = CARTESIAN_POINT ( 'NONE',  ( 58.34606816583844591, 8.411196891453267099, 19.02818770551464667 ) ) ;
#19494 = MECHANICAL_DESIGN_GEOMETRIC_PRESENTATION_REPRESENTATION (  '', ( #2279 ), #19869 ) ;
#19495 = CARTESIAN_POINT ( 'NONE',  ( 69.65000000218496723, 7.499999999999995559, 13.96446609406725692 ) ) ;
#19496 = CARTESIAN_POINT ( 'NONE',  ( 47.23681404676619877, -9.000000000000001776, 5.000000000000079936 ) ) ;
#19497 =( BOUNDED_CURVE ( )  B_SPLINE_CURVE ( 2, ( #4015, #16960, #20768, #13143, #4260, #16602, #14825, #22078, #5697 ),
 .UNSPECIFIED., .F., .F. ) 
 B_SPLINE_CURVE_WITH_KNOTS ( ( 3, 2, 2, 2, 3 ),
 ( 0.06249999999999961836, 0.07812499999999952816, 0.09374999999999943101, 0.1093749999999993339, 0.1249999999999992367 ),
 .UNSPECIFIED. ) 
 CURVE ( )  GEOMETRIC_REPRESENTATION_ITEM ( )  RATIONAL_B_SPLINE_CURVE ( ( 1.000000000000001776, 0.9238795325112848511, 1.000000000000000000, 0.9238795325112867385, 1.000000000000000000, 0.9238795325112867385, 1.000000000000000000, 0.9238795325112904022, 0.9999999999999963363 ) ) 
 REPRESENTATION_ITEM ( '' )  );
#19498 = CARTESIAN_POINT ( 'NONE',  ( -3.355112389629170799, 2.681727112203152963, -0.2256878752776689534 ) ) ;
#19499 = CARTESIAN_POINT ( 'NONE',  ( 68.35000000109246798, 8.538419263543522320, 16.46158073645647235 ) ) ;
#19500 = ORIENTED_EDGE ( 'NONE', *, *, #17394, .T. ) ;
#19501 = AXIS2_PLACEMENT_3D ( 'NONE', #11676, #621, #15268 ) ;
#19502 = DIRECTION ( 'NONE',  ( -0.000000000000000000, -0.000000000000000000, 1.000000000000000000 ) ) ;
#19503 = DIRECTION ( 'NONE',  ( 0.3420201433256622181, -0.9396926207859107594, 0.000000000000000000 ) ) ;
#19504 = FACE_OUTER_BOUND ( 'NONE', #6219, .T. ) ;
#19505 = CARTESIAN_POINT ( 'NONE',  ( 1.872352939448454495E-15, -3.458734125000000770, 18.93750000136560629 ) ) ;
#19506 = VECTOR ( 'NONE', #9913, 1000.000000000000000 ) ;
#19507 = CARTESIAN_POINT ( 'NONE',  ( 4.000000000000000888, 4.898587196589412829E-16, 15.50000000000001066 ) ) ;
#19508 = DIRECTION ( 'NONE',  ( 1.000000000000000000, -0.000000000000000000, -0.000000000000000000 ) ) ;
#19509 = VECTOR ( 'NONE', #6000, 1000.000000000000114 ) ;
#19510 = ORIENTED_EDGE ( 'NONE', *, *, #13206, .F. ) ;
#19511 = CARTESIAN_POINT ( 'NONE',  ( -1.656854249492380804, 4.000000000000000000, -0.8874999999999971800 ) ) ;
#19512 = CARTESIAN_POINT ( 'NONE',  ( 56.90625000000000711, 12.99999999999999645, 13.75735931288070191 ) ) ;
#19513 = DIRECTION ( 'NONE',  ( -0.000000000000000000, -1.000000000000000000, 0.000000000000000000 ) ) ;
#19514 = EDGE_CURVE ( 'NONE', #19393, #18250, #13808, .T. ) ;
#19515 = ORIENTED_EDGE ( 'NONE', *, *, #8797, .T. ) ;
#19516 = CARTESIAN_POINT ( 'NONE',  ( 5.968343123267133343, -4.059728990630809164, -0.4033376246892532713 ) ) ;
#19517 = DIRECTION ( 'NONE',  ( -1.000000000000000000, 0.000000000000000000, 0.000000000000000000 ) ) ;
#19518 = VERTEX_POINT ( 'NONE', #2753 ) ;
#19519 = CARTESIAN_POINT ( 'NONE',  ( 2.000000000000008882, 3.464101615137749945, 0.000000000000000000 ) ) ;
#19520 = ORIENTED_EDGE ( 'NONE', *, *, #1393, .F. ) ;
#19521 = CARTESIAN_POINT ( 'NONE',  ( -2.828427124746189403, 2.828427124746190291, 13.00000000273119660 ) ) ;
#19522 = ORIENTED_EDGE ( 'NONE', *, *, #3329, .F. ) ;
#19523 = CARTESIAN_POINT ( 'NONE',  ( -3.458734124999999437, 0.000000000000000000, 11.68750000136560629 ) ) ;
#19524 = LINE ( 'NONE', #13572, #15359 ) ;
#19525 = AXIS2_PLACEMENT_3D ( 'NONE', #7210, #14639, #14525 ) ;
#19526 = CARTESIAN_POINT ( 'NONE',  ( -67.95000000218495018, 7.499999999999996447, 16.03553390593273775 ) ) ;
#19527 = CARTESIAN_POINT ( 'NONE',  ( 65.75000000109247367, 8.538419263543522320, 16.46158073645647235 ) ) ;
#19528 = CARTESIAN_POINT ( 'NONE',  ( 0.000000000000000000, 0.000000000000000000, 0.000000000000000000 ) ) ;
#19529 = CARTESIAN_POINT ( 'NONE',  ( -68.74999999999998579, 7.499999999999995559, 13.96446609406725692 ) ) ;
#19530 = CARTESIAN_POINT ( 'NONE',  ( -2.344047193898593395, -3.265465875126480455, -1.054683074273691752E-14 ) ) ;
#19531 = CARTESIAN_POINT ( 'NONE',  ( 60.00000000000000711, 12.82842712474617741, 12.17157287525379239 ) ) ;
#19532 =( BOUNDED_CURVE ( )  B_SPLINE_CURVE ( 2, ( #14108, #12560, #8487, #8844, #12201, #23062, #19585, #23542, #3426 ),
 .UNSPECIFIED., .F., .F. ) 
 B_SPLINE_CURVE_WITH_KNOTS ( ( 3, 2, 2, 2, 3 ),
 ( 0.1499999999999999944, 0.1625000000000000056, 0.1749999999999999889, 0.1875000000000000000, 0.2000000000000000111 ),
 .UNSPECIFIED. ) 
 CURVE ( )  GEOMETRIC_REPRESENTATION_ITEM ( )  RATIONAL_B_SPLINE_CURVE ( ( 1.000000000000000000, 0.9238795325112867385, 1.000000000000000000, 0.9238795325112867385, 1.000000000000000000, 0.9238795325112867385, 1.000000000000000000, 0.9238795325112867385, 1.000000000000000000 ) ) 
 REPRESENTATION_ITEM ( '' )  );
#19533 = CARTESIAN_POINT ( 'NONE',  ( -2.117863837641485618E-16, 3.458734125000000770, -1.262499998634402765 ) ) ;
#19534 = DIRECTION ( 'NONE',  ( -0.000000000000000000, -0.000000000000000000, -1.000000000000000000 ) ) ;
#19535 = DIRECTION ( 'NONE',  ( 1.000000000000000000, 0.000000000000000000, 0.000000000000000000 ) ) ;
#19536 = CARTESIAN_POINT ( 'NONE',  ( 2.445694354108821855, -2.445694354108820079, 15.81250000136560629 ) ) ;
#19537 = DIRECTION ( 'NONE',  ( 1.000000000000000000, 7.703719777548943412E-32, 0.000000000000000000 ) ) ;
#19538 = VECTOR ( 'NONE', #7536, 1000.000000000000000 ) ;
#19539 = ORIENTED_EDGE ( 'NONE', *, *, #16152, .T. ) ;
#19540 = CARTESIAN_POINT ( 'NONE',  ( 1.971781867644420635E-15, -4.000000000000000000, 14.37500000273119660 ) ) ;
#19541 = ORIENTED_EDGE ( 'NONE', *, *, #452, .T. ) ;
#19542 = CARTESIAN_POINT ( 'NONE',  ( 59.77893183416158962, 8.411196891453236901, 10.97181229448535511 ) ) ;
#19543 = CARTESIAN_POINT ( 'NONE',  ( -67.95000000109247651, 11.46158073645647235, 16.46158073645647235 ) ) ;
#19544 =( NAMED_UNIT ( * ) PLANE_ANGLE_UNIT ( ) SI_UNIT ( $, .RADIAN. ) );
#19545 = CARTESIAN_POINT ( 'NONE',  ( 4.999999999999999112, 0.000000000000000000, 0.000000000000000000 ) ) ;
#19546 = ORIENTED_EDGE ( 'NONE', *, *, #5585, .T. ) ;
#19547 = DIRECTION ( 'NONE',  ( -0.000000000000000000, -0.000000000000000000, 1.000000000000000000 ) ) ;
#19548 = ORIENTED_EDGE ( 'NONE', *, *, #15956, .T. ) ;
#19549 = DIRECTION ( 'NONE',  ( 1.000000000000000000, 0.000000000000000000, 0.000000000000000000 ) ) ;
#19550 = EDGE_LOOP ( 'NONE', ( #2133, #3901, #9244, #5672 ) ) ;
#19551 = CARTESIAN_POINT ( 'NONE',  ( 55.25231816583843170, 7.926799079670502124, 17.16943976678978245 ) ) ;
#19552 = EDGE_CURVE ( 'NONE', #21603, #2255, #11137, .T. ) ;
#19553 = CARTESIAN_POINT ( 'NONE',  ( -68.95000000218495018, 8.964466094067258695, 12.49999999999999289 ) ) ;
#19554 = DIRECTION ( 'NONE',  ( -0.000000000000000000, -0.000000000000000000, 1.000000000000000000 ) ) ;
#19555 = CARTESIAN_POINT ( 'NONE',  ( 1.432654583217643163, -3.458734124999999882, 17.00000000136560629 ) ) ;
#19556 = CARTESIAN_POINT ( 'NONE',  ( -3.999999999999999112, 1.656854249492380804, 10.06250000273119660 ) ) ;
#19557 = EDGE_CURVE ( 'NONE', #6808, #6494, #22516, .T. ) ;
#19558 = CARTESIAN_POINT ( 'NONE',  ( 57.65625000000002132, 7.000000000000003553, 16.24264068711929099 ) ) ;
#19559 = CARTESIAN_POINT ( 'NONE',  ( 4.000000000000000888, 4.898587196589412829E-16, 17.62500000273119483 ) ) ;
#19560 = CARTESIAN_POINT ( 'NONE',  ( 57.09375000000000711, 11.24264068711927322, 11.99999999999998934 ) ) ;
#19561 = CARTESIAN_POINT ( 'NONE',  ( -2.117863837641485618E-16, 3.458734125000000770, 1.737500001365596347 ) ) ;
#19562 = CARTESIAN_POINT ( 'NONE',  ( 72.50000000000000000, 9.999999999999998224, 12.49999999999999289 ) ) ;
#19563 = DIRECTION ( 'NONE',  ( 0.000000000000000000, -0.000000000000000000, 1.000000000000000000 ) ) ;
#19564 = ORIENTED_EDGE ( 'NONE', *, *, #12329, .F. ) ;
#19565 = LINE ( 'NONE', #3522, #9470 ) ;
#19566 = FACE_OUTER_BOUND ( 'NONE', #8476, .T. ) ;
#19567 = ORIENTED_EDGE ( 'NONE', *, *, #11893, .T. ) ;
#19568 = CARTESIAN_POINT ( 'NONE',  ( 57.84375000000000711, 8.757359312880723223, 18.00000000000000355 ) ) ;
#19569 = CARTESIAN_POINT ( 'NONE',  ( 1.656854249492383024, -3.999999999999999112, -1.262499997268811347 ) ) ;
#19570 = CARTESIAN_POINT ( 'NONE',  ( 1.489200000000000079, 0.000000000000000000, 0.000000000000000000 ) ) ;
#19571 = ORIENTED_EDGE ( 'NONE', *, *, #4507, .T. ) ;
#19572 = VERTEX_POINT ( 'NONE', #8884 ) ;
#19573 = DIRECTION ( 'NONE',  ( -1.000000000000000000, 0.000000000000000000, -0.000000000000000000 ) ) ;
#19574 = DIRECTION ( 'NONE',  ( 1.000000000000000000, 0.000000000000000000, 0.000000000000000000 ) ) ;
#19575 = VERTEX_POINT ( 'NONE', #10574 ) ;
#19576 = DIRECTION ( 'NONE',  ( 1.000000000000000000, 0.000000000000000000, 0.000000000000000000 ) ) ;
#19577 = UNCERTAINTY_MEASURE_WITH_UNIT (LENGTH_MEASURE( 1.000000000000000082E-05 ), #22806, 'distance_accuracy_value', 'NONE');
#19578 = EDGE_CURVE ( 'NONE', #17912, #4980, #4789, .T. ) ;
#19579 = ADVANCED_FACE ( 'NONE', ( #19745, #1190 ), #14274, .T. ) ;
#19580 = VERTEX_POINT ( 'NONE', #5033 ) ;
#19581 = DIRECTION ( 'NONE',  ( 1.000000000000000000, 7.703719777548943412E-32, 0.000000000000000000 ) ) ;
#19582 = CARTESIAN_POINT ( 'NONE',  ( 66.15000000109247935, 8.538419263543524096, 13.53841926354352054 ) ) ;
#19583 = CIRCLE ( 'NONE', #18445, 4.000000000000001776 ) ;
#19584 = ADVANCED_FACE ( 'NONE', ( #23351 ), #17846, .T. ) ;
#19585 = CARTESIAN_POINT ( 'NONE',  ( -2.828427124746188515, -2.828427124746190735, 17.25000000273119838 ) ) ;
#19586 = CYLINDRICAL_SURFACE ( 'NONE', #16073, 4.999999999999999112 ) ;
#19587 = CARTESIAN_POINT ( 'NONE',  ( 51.00000000000000711, 12.82842712474617741, 12.17157287525379239 ) ) ;
#19588 = CARTESIAN_POINT ( 'NONE',  ( -2.445694354108820523, 2.445694354108820523, 3.612500001365594571 ) ) ;
#19589 = CARTESIAN_POINT ( 'NONE',  ( 3.458734125000001214, 1.432654583217640498, 15.00000000136560807 ) ) ;
#19590 = CARTESIAN_POINT ( 'NONE',  ( -0.8800590352214044954, 5.420839058164813373, -19.99999999999999645 ) ) ;
#19591 = CARTESIAN_POINT ( 'NONE',  ( 5.479999999999998650, 0.000000000000000000, 3.059999999999998277 ) ) ;
#19592 = ORIENTED_EDGE ( 'NONE', *, *, #2824, .T. ) ;
#19593 = CARTESIAN_POINT ( 'NONE',  ( 72.50000000000000000, 9.999999999999998224, 14.99999999999999645 ) ) ;
#19594 = FACE_OUTER_BOUND ( 'NONE', #21116, .T. ) ;
#19595 = CARTESIAN_POINT ( 'NONE',  ( -1.600000000000000977, 8.265000000000021885, 0.000000000000000000 ) ) ;
#19596 = VERTEX_POINT ( 'NONE', #12364 ) ;
#19597 = CARTESIAN_POINT ( 'NONE',  ( -66.49999999999998579, 9.999999999999998224, 12.49999999999999289 ) ) ;
#19598 = DIRECTION ( 'NONE',  ( 0.000000000000000000, -0.3090169943749551673, 0.9510565162951511997 ) ) ;
#19599 = EDGE_CURVE ( 'NONE', #7937, #14895, #8413, .T. ) ;
#19600 = CARTESIAN_POINT ( 'NONE',  ( 4.000000000000000888, 4.898587196589412829E-16, 16.50000000000001066 ) ) ;
#19601 = ORIENTED_EDGE ( 'NONE', *, *, #11760, .F. ) ;
#19602 = CARTESIAN_POINT ( 'NONE',  ( 47.85166990323382663, -9.000000000000005329, 5.000000000000079936 ) ) ;
#19603 = EDGE_LOOP ( 'NONE', ( #2569, #19342, #16126, #21969 ) ) ;
#19604 = CARTESIAN_POINT ( 'NONE',  ( 57.78356816583844591, 8.275094609561968184, 11.02818770551464667 ) ) ;
#19605 = ADVANCED_FACE ( 'NONE', ( #1413 ), #14026, .F. ) ;
#19606 = CARTESIAN_POINT ( 'NONE',  ( 67.10000000218495586, 8.232233047033627571, 16.76776695296636532 ) ) ;
#19607 = CARTESIAN_POINT ( 'NONE',  ( 6.500000000000000000, 3.752776749732573247, -3.119443416399232394 ) ) ;
#19608 = CARTESIAN_POINT ( 'NONE',  ( 4.999999999999997335, 5.204748896376250699E-16, -4.250000000000000000 ) ) ;
#19609 = DIRECTION ( 'NONE',  ( -1.000000000000000000, 1.224646799147352714E-16, 0.000000000000000000 ) ) ;
#19610 = ADVANCED_FACE ( 'NONE', ( #1545 ), #8628, .F. ) ;
#19611 = VERTEX_POINT ( 'NONE', #23103 ) ;
#19612 = ADVANCED_FACE ( 'NONE', ( #19275 ), #21535, .F. ) ;
#19613 = CARTESIAN_POINT ( 'NONE',  ( 4.999999999999999112, -9.680994141368810091, 5.222868219166821646 ) ) ;
#19614 = DIRECTION ( 'NONE',  ( -1.000000000000000000, 0.000000000000000000, 0.000000000000000000 ) ) ;
#19615 = CARTESIAN_POINT ( 'NONE',  ( 67.40000000109247935, 10.85617417291294551, 17.06698729999999742 ) ) ;
#19616 = CARTESIAN_POINT ( 'NONE',  ( 1.432654583217641386, 3.458734125000000770, 18.37500000136560274 ) ) ;
#19617 = DIRECTION ( 'NONE',  ( 1.000000000000000000, 0.000000000000000000, 0.000000000000000000 ) ) ;
#19618 = CARTESIAN_POINT ( 'NONE',  ( -12.44420145928343935, -8.974600000000002353, 5.000000000000079936 ) ) ;
#19619 = EDGE_LOOP ( 'NONE', ( #11391, #19510, #6342, #10966 ) ) ;
#19620 = CARTESIAN_POINT ( 'NONE',  ( -2.828427124746189403, -2.828427124746190735, -1.574999999999998179 ) ) ;
#19621 = AXIS2_PLACEMENT_3D ( 'NONE', #11678, #22541, #22413 ) ;
#19622 = CARTESIAN_POINT ( 'NONE',  ( 55.78125000000000711, 8.757359312880703683, 11.99999999999999822 ) ) ;
#19623 = CARTESIAN_POINT ( 'NONE',  ( 1.600000000000004086, 0.000000000000000000, -6.735000000000022524 ) ) ;
#19624 = SURFACE_SIDE_STYLE ('',( #12362 ) ) ;
#19625 = ORIENTED_EDGE ( 'NONE', *, *, #11830, .T. ) ;
#19626 = CARTESIAN_POINT ( 'NONE',  ( 54.99999999999992895, -15.00000000000000000, 1.836970198721037478E-15 ) ) ;
#19627 = CARTESIAN_POINT ( 'NONE',  ( 2.445694354108820079, 2.445694354108820523, -2.637499998634404097 ) ) ;
#19628 = CARTESIAN_POINT ( 'NONE',  ( -66.00000000109245946, 7.933012699999995476, 15.85617417291294196 ) ) ;
#19629 = VECTOR ( 'NONE', #7639, 1000.000000000000000 ) ;
#19630 = VERTEX_POINT ( 'NONE', #2983 ) ;
#19631 = DIRECTION ( 'NONE',  ( 1.000000000000000000, 7.703719777548943412E-32, 0.000000000000000000 ) ) ;
#19632 = ORIENTED_EDGE ( 'NONE', *, *, #19706, .F. ) ;
#19633 = CARTESIAN_POINT ( 'NONE',  ( 1.656854249492381470, 4.000000000000000000, 12.81250000273119660 ) ) ;
#19634 =( BOUNDED_CURVE ( )  B_SPLINE_CURVE ( 2, ( #17064, #18848, #16947, #15055, #15408, #17187, #22310, #11812, #13252 ),
 .UNSPECIFIED., .F., .F. ) 
 B_SPLINE_CURVE_WITH_KNOTS ( ( 3, 2, 2, 2, 3 ),
 ( 0.5000000000000000000, 0.5124999999999999556, 0.5250000000000000222, 0.5374999999999999778, 0.5500000000000000444 ),
 .UNSPECIFIED. ) 
 CURVE ( )  GEOMETRIC_REPRESENTATION_ITEM ( )  RATIONAL_B_SPLINE_CURVE ( ( 1.000000000000000000, 0.9238795325112867385, 1.000000000000000000, 0.9238795325112867385, 1.000000000000000000, 0.9238795325112867385, 1.000000000000000000, 0.9238795325112867385, 1.000000000000000000 ) ) 
 REPRESENTATION_ITEM ( '' )  );
#19635 = ORIENTED_EDGE ( 'NONE', *, *, #15801, .T. ) ;
#19636 = CARTESIAN_POINT ( 'NONE',  ( -2.828427124746189403, 2.828427124746190291, 17.87500000000001066 ) ) ;
#19637 = CARTESIAN_POINT ( 'NONE',  ( -4.000000000000000000, 1.941961291383472732, -0.3515519931180205448 ) ) ;
#19638 = CARTESIAN_POINT ( 'NONE',  ( -68.20000000218495018, 9.999999999999998224, 12.49999999999999289 ) ) ;
#19639 = CARTESIAN_POINT ( 'NONE',  ( 67.10000000109248219, 12.06698729999999919, 15.85617417291294196 ) ) ;
#19640 = EDGE_CURVE ( 'NONE', #23289, #8317, #4780, .T. ) ;
#19641 = DIRECTION ( 'NONE',  ( 1.000000000000000000, 0.000000000000000000, 0.000000000000000000 ) ) ;
#19642 = ADVANCED_FACE ( 'NONE', ( #6829 ), #3347, .T. ) ;
#19643 = CARTESIAN_POINT ( 'NONE',  ( -69.14999999999999147, 12.50000000000000000, 16.03553390593273420 ) ) ;
#19644 = CARTESIAN_POINT ( 'NONE',  ( 4.000000000000000888, 4.898587196589412829E-16, 14.50000000000001066 ) ) ;
#19645 = CARTESIAN_POINT ( 'NONE',  ( 59.99999999999729994, 11.15626659836185119, 18.14511749203898106 ) ) ;
#19646 = CARTESIAN_POINT ( 'NONE',  ( -3.458734125000000770, 0.000000000000000000, -0.01249999863440348635 ) ) ;
#19647 = DIRECTION ( 'NONE',  ( 0.000000000000000000, 0.000000000000000000, 1.000000000000000000 ) ) ;
#19648 = CARTESIAN_POINT ( 'NONE',  ( -20.00000000000000711, 1.500000000000003109, -17.32050807568892736 ) ) ;
#19649 = CARTESIAN_POINT ( 'NONE',  ( 1.872352939448454495E-15, -3.458734125000000326, 18.68750000136560629 ) ) ;
#19650 = CARTESIAN_POINT ( 'NONE',  ( -6.500000000000000000, 3.752776749732564809, -3.700000000000000178 ) ) ;
#19651 = EDGE_LOOP ( 'NONE', ( #10508, #1408, #14213, #8420 ) ) ;
#19652 = CARTESIAN_POINT ( 'NONE',  ( 14.99999999999995559, -15.00000000000000000, -50.00000000000000000 ) ) ;
#19653 = ORIENTED_EDGE ( 'NONE', *, *, #10631, .F. ) ;
#19654 = CARTESIAN_POINT ( 'NONE',  ( 54.24768183416157541, 7.830560233210222876, 17.07320092032950498 ) ) ;
#19655 = CARTESIAN_POINT ( 'NONE',  ( -66.45000000109247651, 9.999999999999998224, 17.06698730000000097 ) ) ;
#19656 = CARTESIAN_POINT ( 'NONE',  ( 0.000000000000000000, 0.000000000000000000, 0.000000000000000000 ) ) ;
#19657 = CARTESIAN_POINT ( 'NONE',  ( 3.458734125000000326, 4.235727675282971730E-16, -1.762499998634403209 ) ) ;
#19658 = VERTEX_POINT ( 'NONE', #17501 ) ;
#19659 = DIRECTION ( 'NONE',  ( 0.000000000000000000, 0.000000000000000000, -1.000000000000000000 ) ) ;
#19660 = VECTOR ( 'NONE', #7725, 1000.000000000000114 ) ;
#19661 = ORIENTED_EDGE ( 'NONE', *, *, #7795, .F. ) ;
#19662 = FACE_OUTER_BOUND ( 'NONE', #19550, .T. ) ;
#19663 = VERTEX_POINT ( 'NONE', #1071 ) ;
#19664 = CARTESIAN_POINT ( 'NONE',  ( 53.84606816583843880, 8.825410453826357582, 18.02818770551464667 ) ) ;
#19665 = AXIS2_PLACEMENT_3D ( 'NONE', #3990, #13239, #9525 ) ;
#19666 = CARTESIAN_POINT ( 'NONE',  ( -67.80000000218494449, 9.999999999999998224, 17.49999999999999645 ) ) ;
#19667 = FACE_OUTER_BOUND ( 'NONE', #11126, .T. ) ;
#19668 = CARTESIAN_POINT ( 'NONE',  ( 0.7185353092834488864, -8.974600000000002353, 5.000000000000079936 ) ) ;
#19669 = CARTESIAN_POINT ( 'NONE',  ( -1.432654583217639166, 3.458734125000000770, 16.50000000136560629 ) ) ;
#19670 = DIRECTION ( 'NONE',  ( 1.000000000000000000, 0.000000000000000000, -0.000000000000000000 ) ) ;
#19671 = CARTESIAN_POINT ( 'NONE',  ( 56.15625000000002132, 7.000000000000003553, 16.24264068711929099 ) ) ;
#19672 = FACE_OUTER_BOUND ( 'NONE', #17534, .T. ) ;
#19673 = CARTESIAN_POINT ( 'NONE',  ( 58.59375000000000711, 11.24264068711927322, 11.99999999999998934 ) ) ;
#19674 = CARTESIAN_POINT ( 'NONE',  ( 1.432654583217642275, -3.458734124999999882, 0.3000000013655960696 ) ) ;
#19675 = CARTESIAN_POINT ( 'NONE',  ( 0.9097406175788815830, -3.344736155888329510, 2.040000000000001812 ) ) ;
#19676 = CARTESIAN_POINT ( 'NONE',  ( 20.55500000000001748, 0.000000000000000000, 0.000000000000000000 ) ) ;
#19677 = EDGE_CURVE ( 'NONE', #21587, #22281, #19350, .T. ) ;
#19678 = ORIENTED_EDGE ( 'NONE', *, *, #12732, .F. ) ;
#19679 = CARTESIAN_POINT ( 'NONE',  ( 27.50000000000000000, 7.500000000000001776, -31.01025403784447221 ) ) ;
#19680 = CARTESIAN_POINT ( 'NONE',  ( -4.140404888673278272, -2.228338276487456415, -3.686887068327035166 ) ) ;
#19681 = EDGE_LOOP ( 'NONE', ( #12952, #16725, #9213, #21659, #8274, #8237 ) ) ;
#19682 = CARTESIAN_POINT ( 'NONE',  ( 59.81250000000000711, 13.00000000000000000, 14.99999999999998757 ) ) ;
#19683 = VECTOR ( 'NONE', #7014, 1000.000000000000000 ) ;
#19684 = CARTESIAN_POINT ( 'NONE',  ( 1.656854249492380360, 4.000000000000000000, 0.1125000027311862244 ) ) ;
#19685 = AXIS2_PLACEMENT_3D ( 'NONE', #11289, #16546, #3710 ) ;
#19686 = DIRECTION ( 'NONE',  ( 1.000000000000000000, 0.000000000000000000, 0.000000000000000000 ) ) ;
#19687 = EDGE_LOOP ( 'NONE', ( #12412, #23439, #16589, #281 ) ) ;
#19688 = ORIENTED_EDGE ( 'NONE', *, *, #7023, .F. ) ;
#19689 = DIRECTION ( 'NONE',  ( -1.000000000000000000, -0.000000000000000000, -0.000000000000000000 ) ) ;
#19690 = LINE ( 'NONE', #4982, #13724 ) ;
#19691 = VERTEX_POINT ( 'NONE', #8637 ) ;
#19692 = SURFACE_STYLE_USAGE ( .BOTH. , #21130 ) ;
#19693 = CARTESIAN_POINT ( 'NONE',  ( -69.70000000218495018, 8.232233047033629347, 13.23223304703362402 ) ) ;
#19694 = ORIENTED_EDGE ( 'NONE', *, *, #5896, .T. ) ;
#19695 = DIRECTION ( 'NONE',  ( -1.000000000000000000, 0.000000000000000000, 0.000000000000000000 ) ) ;
#19696 = VECTOR ( 'NONE', #19686, 1000.000000000000000 ) ;
#19697 = CARTESIAN_POINT ( 'NONE',  ( 71.14999999999999147, 7.499999999999995559, 13.96446609406725692 ) ) ;
#19698 = AXIS2_PLACEMENT_3D ( 'NONE', #2717, #914, #4640 ) ;
#19699 = FACE_OUTER_BOUND ( 'NONE', #21385, .T. ) ;
#19700 = DIRECTION ( 'NONE',  ( 0.000000000000000000, 0.000000000000000000, 1.000000000000000000 ) ) ;
#19701 = CARTESIAN_POINT ( 'NONE',  ( 58.81481816583843170, 14.00000000000000178, 14.93194885905434610 ) ) ;
#19702 = FILL_AREA_STYLE ('',( #12438 ) ) ;
#19703 = CARTESIAN_POINT ( 'NONE',  ( -3.458734124999998993, 0.000000000000000000, 16.43750000136560629 ) ) ;
#19704 = CARTESIAN_POINT ( 'NONE',  ( 14.11308378033275446, -11.25000000000000355, 5.000000000000079936 ) ) ;
#19705 = AXIS2_PLACEMENT_3D ( 'NONE', #12572, #17814, #1514 ) ;
#19706 = EDGE_CURVE ( 'NONE', #19663, #15405, #4026, .T. ) ;
#19707 = CARTESIAN_POINT ( 'NONE',  ( 41.55923975928345016, -8.974600000000002353, 5.000000000000079936 ) ) ;
#19708 = ORIENTED_EDGE ( 'NONE', *, *, #14204, .F. ) ;
#19709 = DIRECTION ( 'NONE',  ( 1.000000000000000000, -0.000000000000000000, -0.000000000000000000 ) ) ;
#19710 = EDGE_CURVE ( 'NONE', #872, #3547, #15521, .T. ) ;
#19711 = CARTESIAN_POINT ( 'NONE',  ( 68.14999999999999147, 11.03553390593273420, 12.49999999999998934 ) ) ;
#19712 = CARTESIAN_POINT ( 'NONE',  ( 4.999999999999999112, 6.807171995660585395, 6.478011392632914145 ) ) ;
#19713 = ORIENTED_EDGE ( 'NONE', *, *, #8366, .F. ) ;
#19714 = FACE_OUTER_BOUND ( 'NONE', #12016, .T. ) ;
#19715 = CARTESIAN_POINT ( 'NONE',  ( 4.999999999999999112, 0.000000000000000000, 0.000000000000000000 ) ) ;
#19716 = CIRCLE ( 'NONE', #22781, 6.760799999999997034 ) ;
#19717 = AXIS2_PLACEMENT_3D ( 'NONE', #20658, #18628, #18755 ) ;
#19718 = VERTEX_POINT ( 'NONE', #20090 ) ;
#19719 = EDGE_CURVE ( 'NONE', #3801, #9962, #9006, .T. ) ;
#19720 = CARTESIAN_POINT ( 'NONE',  ( -4.000000000000000000, 0.000000000000000000, -0.6999999999999975131 ) ) ;
#19721 = EDGE_LOOP ( 'NONE', ( #22016, #21176, #45, #21450 ) ) ;
#19722 = DIRECTION ( 'NONE',  ( 1.000000000000000000, -0.000000000000000000, -0.000000000000000000 ) ) ;
#19723 = ORIENTED_EDGE ( 'NONE', *, *, #943, .T. ) ;
#19724 = CARTESIAN_POINT ( 'NONE',  ( 54.56250000000000711, 5.999999999999996447, 15.00000000000001599 ) ) ;
#19725 = CARTESIAN_POINT ( 'NONE',  ( 68.70000000218495018, 8.232233047033627571, 16.76776695296636532 ) ) ;
#19726 = CARTESIAN_POINT ( 'NONE',  ( 7.000000000000000000, 0.000000000000000000, 5.000000000000007994 ) ) ;
#19727 = CARTESIAN_POINT ( 'NONE',  ( 2.500000000000000000, 1.178949249685212974, -2.042000000000001148 ) ) ;
#19728 = CARTESIAN_POINT ( 'NONE',  ( -3.999999999999999112, 0.000000000000000000, 21.31370849898476649 ) ) ;
#19729 = ORIENTED_EDGE ( 'NONE', *, *, #2671, .F. ) ;
#19730 = DIRECTION ( 'NONE',  ( 0.000000000000000000, 0.000000000000000000, 1.000000000000000000 ) ) ;
#19731 = CARTESIAN_POINT ( 'NONE',  ( 60.52893183416158251, 11.58880310854676132, 19.02818770551463956 ) ) ;
#19732 = ADVANCED_FACE ( 'NONE', ( #9462 ), #20211, .T. ) ;
#19733 = CARTESIAN_POINT ( 'NONE',  ( 2.828427124746190735, -2.828427124746189847, -1.199999997268811125 ) ) ;
#19734 = DIRECTION ( 'NONE',  ( 1.224646799147353207E-16, 0.000000000000000000, 1.000000000000000000 ) ) ;
#19735 = CARTESIAN_POINT ( 'NONE',  ( -3.458734124999999437, 1.432654583217640498, 17.62500000136560274 ) ) ;
#19736 = PLANE ( 'NONE',  #13599 ) ;
#19737 = EDGE_CURVE ( 'NONE', #16212, #15725, #7675, .T. ) ;
#19738 = CARTESIAN_POINT ( 'NONE',  ( 4.999999999999999112, 1.975651141462391402, -10.82112760146734054 ) ) ;
#19739 = ORIENTED_EDGE ( 'NONE', *, *, #18587, .T. ) ;
#19740 = CARTESIAN_POINT ( 'NONE',  ( -0.3925654445992010633, 3.441971588417507721, -3.295601554149321988 ) ) ;
#19741 = EDGE_CURVE ( 'NONE', #2131, #22090, #7545, .T. ) ;
#19742 = CARTESIAN_POINT ( 'NONE',  ( 57.56250000000000000, 6.999999999999997335, 15.00000000000000533 ) ) ;
#19743 = CARTESIAN_POINT ( 'NONE',  ( 66.59999999999999432, 11.76776695296636888, 13.23223304703362579 ) ) ;
#19744 = ORIENTED_EDGE ( 'NONE', *, *, #9529, .T. ) ;
#19745 = FACE_OUTER_BOUND ( 'NONE', #23615, .T. ) ;
#19746 = CARTESIAN_POINT ( 'NONE',  ( 6.353591512924457348E-16, -3.458734125000000326, -1.012499998634402543 ) ) ;
#19747 = CARTESIAN_POINT ( 'NONE',  ( -2.688821387764050996E-14, -4.618802153517012954, -0.4999999999999995559 ) ) ;
#19748 = EDGE_CURVE ( 'NONE', #8094, #21424, #11489, .T. ) ;
#19749 = ORIENTED_EDGE ( 'NONE', *, *, #13319, .T. ) ;
#19750 = CARTESIAN_POINT ( 'NONE',  ( -65.80000000218494449, 9.999999999999998224, 12.49999999999999289 ) ) ;
#19751 = ORIENTED_EDGE ( 'NONE', *, *, #15839, .T. ) ;
#19752 = ADVANCED_FACE ( 'NONE', ( #3820 ), #9348, .T. ) ;
#19753 = DIRECTION ( 'NONE',  ( 1.000000000000000000, 0.000000000000000000, -1.445602896647339163E-16 ) ) ;
#19754 = EDGE_LOOP ( 'NONE', ( #7406, #3199 ) ) ;
#19755 = CARTESIAN_POINT ( 'NONE',  ( 1.656854249492384135, -3.999999999999999112, 19.31250000000001776 ) ) ;
#19756 = CARTESIAN_POINT ( 'NONE',  ( -66.09999999999999432, 9.999999999999998224, 17.49999999999999645 ) ) ;
#19757 = CARTESIAN_POINT ( 'NONE',  ( -1.656854249492379472, 4.000000000000000000, 10.81250000000001243 ) ) ;
#19758 = FACE_OUTER_BOUND ( 'NONE', #16408, .T. ) ;
#19759 = CARTESIAN_POINT ( 'NONE',  ( 27.50000000000000000, 1.500000000000003109, -31.01025403784446510 ) ) ;
#19760 = CARTESIAN_POINT ( 'NONE',  ( -67.70000000000000284, 9.999999999999998224, 17.49999999999999645 ) ) ;
#19761 = CARTESIAN_POINT ( 'NONE',  ( 0.000000000000000000, 0.000000000000000000, -4.000000000000000000 ) ) ;
#19762 = CARTESIAN_POINT ( 'NONE',  ( 60.00000000000001421, 13.04648002170960197, 12.38962577221721340 ) ) ;
#19763 = CIRCLE ( 'NONE', #17503, 4.000000000000001776 ) ;
#19764 = CARTESIAN_POINT ( 'NONE',  ( 2.445694354108820967, -2.445694354108820079, -0.6374999986344023206 ) ) ;
#19765 = CARTESIAN_POINT ( 'NONE',  ( -67.50000000218494733, 11.76776695296636888, 13.23223304703362579 ) ) ;
#19766 = ADVANCED_FACE ( 'NONE', ( #16636 ), #14746, .F. ) ;
#19767 = CARTESIAN_POINT ( 'NONE',  ( 67.70000000000000284, 9.999999999999998224, 17.49999999999999645 ) ) ;
#19768 = CARTESIAN_POINT ( 'NONE',  ( 3.458734125000002102, -1.432654583217639610, 16.87500000136560629 ) ) ;
#19769 = CARTESIAN_POINT ( 'NONE',  ( -66.50000000218494733, 8.232233047033629347, 13.23223304703362402 ) ) ;
#19770 = VERTEX_POINT ( 'NONE', #7199 ) ;
#19771 = AXIS2_PLACEMENT_3D ( 'NONE', #3270, #5184, #21573 ) ;
#19772 = CARTESIAN_POINT ( 'NONE',  ( -71.65000000109247935, 9.999999999999998224, 12.93301269999999192 ) ) ;
#19773 = ORIENTED_EDGE ( 'NONE', *, *, #14484, .F. ) ;
#19774 = CARTESIAN_POINT ( 'NONE',  ( 54.62268183416157541, 12.78030770151606177, 17.87654654797631792 ) ) ;
#19775 = CARTESIAN_POINT ( 'NONE',  ( -68.65000000109247935, 12.06698730000000097, 14.99999999999999645 ) ) ;
#19776 = ADVANCED_FACE ( 'NONE', ( #5742 ), #18315, .F. ) ;
#19777 =( BOUNDED_SURFACE ( )  B_SPLINE_SURFACE ( 3, 2, ( 
 ( #10273, #15999, #19682, #17447, #21353, #8474, #19805, #13975, #1241, #1482, #8824, #12182, #10398, #17788, #3287, #5083, #8579, #15885, #7011, #6772, #14088, #6894, #10629, #19568, #21588, #3162, #1360, #14214, #5202, #12542, #16697, #18483, #7379, #7488, #5554, #14931, #19925, #159, #9406, #14806, #16467, #273, #9056, #23644, #5673, #5324, #18246, #7608, #1601, #11088, #22184, #20386, #12667, #18135, #16347, #5798, #13126, #14447, #10970, #3631, #14687, #12776, #8941, #20028, #20142, #2066, #10752, #18025, #21839, #1713, #21944, #3747, #16233, #23519, #18372, #3875, #7133, #21712, #7257, #3525, #10858, #14573, #1953, #5440, #12886, #9291, #1831, #9182, #22055, #20271, #46, #16580, #13006, #11209, #22552, #13710, #13591 ),
 ( #2427, #17176, #20857, #6159, #8091, #18604, #4349, #11574, #9758, #6274, #10011, #11806, #630, #758, #13482, #8199, #13241, #15400, #2668, #22664, #17056, #17299, #2317, #16940, #4464, #22302, #18842, #864, #2189, #11686, #15512, #3992, #5915, #11452, #9650, #22780, #6389, #7732, #4237, #20629, #7960, #6035, #9527, #15280, #20743, #11332, #18955, #16825, #2540, #18727, #403, #15044, #13361, #20508, #4113, #9884, #517, #19076, #7839, #15160, #22421, #19302, #23023, #23249, #8668, #8551, #3013, #2893, #15753, #1328, #21320, #21204, #19654, #1449, #8786, #17532, #6858, #10241, #8310, #15858, #5056, #4818, #6745, #14052, #20971, #15633, #15966, #23378, #12276, #4592, #6981, #10365, #4706, #11927, #19196, #6628, #22902 ),
 ( #23132, #3137, #6518, #1097, #8443, #13948, #14183, #21443, #4940, #17654, #12150, #19417, #12389, #19542, #1214, #3255, #16091, #2780, #10479, #10602, #17760, #13837, #17876, #10120, #17413, #982, #21092, #12039, #8910, #1927, #16670, #5526, #21560, #14659, #9379, #21, #9153, #22029, #3719, #12860, #14777, #16556, #12980, #3378, #5646, #10718, #12638, #20116, #132, #16325, #10944, #1572, #11061, #9269, #244, #18223, #16205, #14299, #5173, #14546, #20244, #3851, #12514, #19897, #7354, #7461, #11186, #5295, #19774, #18460, #17995, #12751, #18347, #2041, #16439, #23491, #7104, #21916, #21812, #20003, #14421, #21684, #3499, #1806, #10834, #18108, #1688, #9032, #23616, #7230, #5414, #3605, #18932, #15022, #22276, #15251, #11301 ),
 ( #11549, #2518, #15374, #18575, #16792, #5889, #9852, #17149, #3965, #2287, #18697, #15134, #4084, #14898, #493, #16916, #11664, #6007, #22518, #727, #8060, #7705, #4208, #2156, #13332, #18818, #5774, #13101, #605, #7579, #372, #22155, #20357, #9493, #13213, #7931, #20482, #6128, #11422, #9625, #7816, #22397, #20600, #2403, #9735, #17030, #13457, #20719, #4323, #3202, #21633, #18061, #17825, #12457, #3091, #14369, #10787, #1757, #19724, #17714, #18174, #6691, #16040, #16274, #23566, #14009, #14130, #8862, #1641, #3449, #6809, #15811, #21752, #23083, #14254, #5238, #8986, #10666, #19842, #21267, #16159, #23328, #21511, #7173, #5363, #14489, #3321, #12582, #17942, #19959, #1277, #12707, #3559, #10896, #5122, #4887, #21396 ),
 ( #10549, #12225, #1523, #6939, #8614, #23446, #7051, #19493, #10433, #15918, #23196, #5014, #12343, #19604, #1391, #8732, #5832, #9094, #18643, #14843, #18288, #7414, #16387, #79, #440, #11243, #5953, #22221, #16617, #18409, #5715, #1872, #15084, #9220, #22097, #9572, #14609, #7764, #1986, #20185, #18517, #3792, #7301, #196, #9441, #22339, #11132, #14970, #11366, #9325, #13047, #20069, #7651, #4031, #18770, #20306, #11007, #11497, #23685, #7526, #16865, #13278, #21870, #14723, #2103, #2228, #20421, #21981, #5476, #20547, #12811, #3907, #13160, #4151, #16735, #3671, #16503, #317, #5598, #12924, #4952, #8677, #10490, #23032, #23143, #21214, #6872, #11940, #15869, #1341, #6754, #8454, #15977, #993, #15641, #21332, #20983 ),
 ( #3024, #23262, #12400, #4604, #10133, #8318, #14195, #21453, #6400, #2904, #19313, #6642, #4716, #17308, #15761, #1107, #5066, #13956, #2682, #4828, #17426, #875, #8209, #12047, #19205, #10021, #17539, #22792, #12160, #8561, #2791, #6527, #22913, #10250, #12287, #14066, #19428, #10375, #13846, #21101, #19551, #17662, #1223, #15526, #13720, #3146, #17770, #21926, #8922, #6990, #7238, #3729, #3508, #5422, #12759, #19664, #14310, #7361, #22037, #10953, #3267, #20013, #14790, #3613, #14556, #11070, #9162, #18230, #20123, #5535, #18355, #5305, #1936, #9277, #10843, #1814, #16450, #10613, #21569, #14667, #5654, #31, #17884, #12870, #1459, #16562, #21821, #140, #7469, #8802, #16104, #23388, #5182, #12647, #12524, #19786, #7115 ),
 ( #16331, #3386, #10730, #18007, #1583, #23625, #16215, #23500, #14430, #19906, #21695, #18119, #1695, #9039, #6015, #7941, #616, #3975, #15385, #18940, #20253, #11434, #2411, #6141, #7824, #17038, #3859, #13342, #20491, #18708, #15261, #2525, #20727, #9634, #9744, #15143, #17159, #22164, #22530, #11671, #13467, #2297, #9862, #11309, #2166, #4331, #9505, #18826, #738, #16924, #13223, #5781, #501, #22407, #11557, #8070, #11194, #22649, #253, #18585, #7588, #12988, #22283, #18469, #2047, #9387, #20609, #13109, #16802, #16681, #382, #14906, #4219, #20367, #7714, #4092, #5900, #15029, #15495, #12257, #6376, #12018, #6724, #11785, #21299, #15615, #17395, #15735, #962, #4450, #13818, #6613, #1198, #10462, #1310, #4574, #23007 ) ),
 .UNSPECIFIED., .T., .F., .F. ) 
 B_SPLINE_SURFACE_WITH_KNOTS ( ( 4, 3, 4 ),
 ( 3, 2, 2, 2, 2, 2, 2, 2, 2, 2, 2, 2, 2, 2, 2, 2, 2, 2, 2, 2, 2, 2, 2, 2, 2, 2, 2, 2, 2, 2, 2, 2, 2, 2, 2, 2, 2, 2, 2, 2, 2, 2, 2, 2, 2, 2, 2, 2, 3 ),
 ( 0.000000000000000000, 0.5000000000000000000, 1.000000000000000000 ),
 ( 0.000000000000000000, 0.02083333333333333218, 0.04166666666666666435, 0.06250000000000000000, 0.08333333333333332871, 0.1041666666666666713, 0.1250000000000000000, 0.1458333333333333426, 0.1666666666666666574, 0.1875000000000000000, 0.2083333333333333426, 0.2291666666666666574, 0.2500000000000000000, 0.2708333333333333148, 0.2916666666666666852, 0.3125000000000000000, 0.3333333333333333148, 0.3541666666666666852, 0.3750000000000000000, 0.3958333333333333148, 0.4166666666666666852, 0.4375000000000000000, 0.4583333333333333148, 0.4791666666666666852, 0.5000000000000000000, 0.5208333333333333703, 0.5416666666666666297, 0.5625000000000000000, 0.5833333333333333703, 0.6041666666666666297, 0.6250000000000000000, 0.6458333333333333703, 0.6666666666666666297, 0.6875000000000000000, 0.7083333333333333703, 0.7291666666666666297, 0.7500000000000000000, 0.7708333333333333703, 0.7916666666666666297, 0.8125000000000000000, 0.8333333333333333703, 0.8541666666666666297, 0.8750000000000000000, 0.8958333333333333703, 0.9166666666666666297, 0.9375000000000000000, 0.9583333333333333703, 0.9791666666666666297, 1.000000000000000000 ),
 .UNSPECIFIED. ) 
 GEOMETRIC_REPRESENTATION_ITEM ( )  RATIONAL_B_SPLINE_SURFACE ( (
 ( 1.000000000000000000, 0.9238795325112867385, 1.000000000000000000, 0.9238795325112867385, 1.000000000000000000, 0.9238795325112867385, 1.000000000000000000, 0.9238795325112867385, 1.000000000000000000, 0.9238795325112867385, 1.000000000000000000, 0.9238795325112867385, 1.000000000000000000, 0.9238795325112867385, 1.000000000000000000, 0.9238795325112867385, 1.000000000000000000, 0.9238795325112867385, 1.000000000000000000, 0.9238795325112867385, 1.000000000000000000, 0.9238795325112867385, 1.000000000000000000, 0.9238795325112867385, 1.000000000000000000, 0.9238795325112867385, 1.000000000000000000, 0.9238795325112867385, 1.000000000000000000, 0.9238795325112867385, 1.000000000000000000, 0.9238795325112867385, 1.000000000000000000, 0.9238795325112867385, 1.000000000000000000, 0.9238795325112867385, 1.000000000000000000, 0.9238795325112867385, 1.000000000000000000, 0.9238795325112867385, 1.000000000000000000, 0.9238795325112867385, 1.000000000000000000, 0.9238795325112867385, 1.000000000000000000, 0.9238795325112867385, 1.000000000000000000, 0.9238795325112867385, 1.000000000000000000, 0.9238795325112867385, 1.000000000000000000, 0.9238795325112867385, 1.000000000000000000, 0.9238795325112867385, 1.000000000000000000, 0.9238795325112867385, 1.000000000000000000, 0.9238795325112867385, 1.000000000000000000, 0.9238795325112867385, 1.000000000000000000, 0.9238795325112867385, 1.000000000000000000, 0.9238795325112867385, 1.000000000000000000, 0.9238795325112867385, 1.000000000000000000, 0.9238795325112867385, 1.000000000000000000, 0.9238795325112867385, 1.000000000000000000, 0.9238795325112867385, 1.000000000000000000, 0.9238795325112867385, 1.000000000000000000, 0.9238795325112867385, 1.000000000000000000, 0.9238795325112867385, 1.000000000000000000, 0.9238795325112867385, 1.000000000000000000, 0.9238795325112867385, 1.000000000000000000, 0.9238795325112867385, 1.000000000000000000, 0.9238795325112867385, 1.000000000000000000, 0.9238795325112867385, 1.000000000000000000, 0.9238795325112867385, 1.000000000000000000, 0.9238795325112867385, 1.000000000000000000, 0.9238795325112867385, 1.000000000000000000, 0.9238795325112867385, 1.000000000000000000),
 ( 0.3333333333333333703, 0.3079598441704289313, 0.3333333333333333703, 0.3079598441704289313, 0.3333333333333333703, 0.3079598441704289313, 0.3333333333333333703, 0.3079598441704289313, 0.3333333333333333703, 0.3079598441704289313, 0.3333333333333333703, 0.3079598441704289313, 0.3333333333333333703, 0.3079598441704289313, 0.3333333333333333703, 0.3079598441704289313, 0.3333333333333333703, 0.3079598441704289313, 0.3333333333333333703, 0.3079598441704289313, 0.3333333333333333703, 0.3079598441704289313, 0.3333333333333333703, 0.3079598441704289313, 0.3333333333333333703, 0.3079598441704289313, 0.3333333333333333703, 0.3079598441704289313, 0.3333333333333333703, 0.3079598441704289313, 0.3333333333333333703, 0.3079598441704289313, 0.3333333333333333703, 0.3079598441704289313, 0.3333333333333333703, 0.3079598441704289313, 0.3333333333333333703, 0.3079598441704289313, 0.3333333333333333703, 0.3079598441704289313, 0.3333333333333333703, 0.3079598441704289313, 0.3333333333333333703, 0.3079598441704289313, 0.3333333333333333703, 0.3079598441704289313, 0.3333333333333333703, 0.3079598441704289313, 0.3333333333333333703, 0.3079598441704289313, 0.3333333333333333703, 0.3079598441704289313, 0.3333333333333333703, 0.3079598441704289313, 0.3333333333333333703, 0.3079598441704289313, 0.3333333333333333703, 0.3079598441704289313, 0.3333333333333333703, 0.3079598441704289313, 0.3333333333333333703, 0.3079598441704289313, 0.3333333333333333703, 0.3079598441704289313, 0.3333333333333333703, 0.3079598441704289313, 0.3333333333333333703, 0.3079598441704289313, 0.3333333333333333703, 0.3079598441704289313, 0.3333333333333333703, 0.3079598441704289313, 0.3333333333333333703, 0.3079598441704289313, 0.3333333333333333703, 0.3079598441704289313, 0.3333333333333333703, 0.3079598441704289313, 0.3333333333333333703, 0.3079598441704289313, 0.3333333333333333703, 0.3079598441704289313, 0.3333333333333333703, 0.3079598441704289313, 0.3333333333333333703, 0.3079598441704289313, 0.3333333333333333703, 0.3079598441704289313, 0.3333333333333333703, 0.3079598441704289313, 0.3333333333333333703, 0.3079598441704289313, 0.3333333333333333703, 0.3079598441704289313, 0.3333333333333333703, 0.3079598441704289313, 0.3333333333333333703),
 ( 0.3333333333333333703, 0.3079598441704289313, 0.3333333333333333703, 0.3079598441704289313, 0.3333333333333333703, 0.3079598441704289313, 0.3333333333333333703, 0.3079598441704289313, 0.3333333333333333703, 0.3079598441704289313, 0.3333333333333333703, 0.3079598441704289313, 0.3333333333333333703, 0.3079598441704289313, 0.3333333333333333703, 0.3079598441704289313, 0.3333333333333333703, 0.3079598441704289313, 0.3333333333333333703, 0.3079598441704289313, 0.3333333333333333703, 0.3079598441704289313, 0.3333333333333333703, 0.3079598441704289313, 0.3333333333333333703, 0.3079598441704289313, 0.3333333333333333703, 0.3079598441704289313, 0.3333333333333333703, 0.3079598441704289313, 0.3333333333333333703, 0.3079598441704289313, 0.3333333333333333703, 0.3079598441704289313, 0.3333333333333333703, 0.3079598441704289313, 0.3333333333333333703, 0.3079598441704289313, 0.3333333333333333703, 0.3079598441704289313, 0.3333333333333333703, 0.3079598441704289313, 0.3333333333333333703, 0.3079598441704289313, 0.3333333333333333703, 0.3079598441704289313, 0.3333333333333333703, 0.3079598441704289313, 0.3333333333333333703, 0.3079598441704289313, 0.3333333333333333703, 0.3079598441704289313, 0.3333333333333333703, 0.3079598441704289313, 0.3333333333333333703, 0.3079598441704289313, 0.3333333333333333703, 0.3079598441704289313, 0.3333333333333333703, 0.3079598441704289313, 0.3333333333333333703, 0.3079598441704289313, 0.3333333333333333703, 0.3079598441704289313, 0.3333333333333333703, 0.3079598441704289313, 0.3333333333333333703, 0.3079598441704289313, 0.3333333333333333703, 0.3079598441704289313, 0.3333333333333333703, 0.3079598441704289313, 0.3333333333333333703, 0.3079598441704289313, 0.3333333333333333703, 0.3079598441704289313, 0.3333333333333333703, 0.3079598441704289313, 0.3333333333333333703, 0.3079598441704289313, 0.3333333333333333703, 0.3079598441704289313, 0.3333333333333333703, 0.3079598441704289313, 0.3333333333333333703, 0.3079598441704289313, 0.3333333333333333703, 0.3079598441704289313, 0.3333333333333333703, 0.3079598441704289313, 0.3333333333333333703, 0.3079598441704289313, 0.3333333333333333703, 0.3079598441704289313, 0.3333333333333333703, 0.3079598441704289313, 0.3333333333333333703),
 ( 1.000000000000000000, 0.9238795325112867385, 1.000000000000000000, 0.9238795325112867385, 1.000000000000000000, 0.9238795325112867385, 1.000000000000000000, 0.9238795325112867385, 1.000000000000000000, 0.9238795325112867385, 1.000000000000000000, 0.9238795325112867385, 1.000000000000000000, 0.9238795325112867385, 1.000000000000000000, 0.9238795325112867385, 1.000000000000000000, 0.9238795325112867385, 1.000000000000000000, 0.9238795325112867385, 1.000000000000000000, 0.9238795325112867385, 1.000000000000000000, 0.9238795325112867385, 1.000000000000000000, 0.9238795325112867385, 1.000000000000000000, 0.9238795325112867385, 1.000000000000000000, 0.9238795325112867385, 1.000000000000000000, 0.9238795325112867385, 1.000000000000000000, 0.9238795325112867385, 1.000000000000000000, 0.9238795325112867385, 1.000000000000000000, 0.9238795325112867385, 1.000000000000000000, 0.9238795325112867385, 1.000000000000000000, 0.9238795325112867385, 1.000000000000000000, 0.9238795325112867385, 1.000000000000000000, 0.9238795325112867385, 1.000000000000000000, 0.9238795325112867385, 1.000000000000000000, 0.9238795325112867385, 1.000000000000000000, 0.9238795325112867385, 1.000000000000000000, 0.9238795325112867385, 1.000000000000000000, 0.9238795325112867385, 1.000000000000000000, 0.9238795325112867385, 1.000000000000000000, 0.9238795325112867385, 1.000000000000000000, 0.9238795325112867385, 1.000000000000000000, 0.9238795325112867385, 1.000000000000000000, 0.9238795325112867385, 1.000000000000000000, 0.9238795325112867385, 1.000000000000000000, 0.9238795325112867385, 1.000000000000000000, 0.9238795325112867385, 1.000000000000000000, 0.9238795325112867385, 1.000000000000000000, 0.9238795325112867385, 1.000000000000000000, 0.9238795325112867385, 1.000000000000000000, 0.9238795325112867385, 1.000000000000000000, 0.9238795325112867385, 1.000000000000000000, 0.9238795325112867385, 1.000000000000000000, 0.9238795325112867385, 1.000000000000000000, 0.9238795325112867385, 1.000000000000000000, 0.9238795325112867385, 1.000000000000000000, 0.9238795325112867385, 1.000000000000000000, 0.9238795325112867385, 1.000000000000000000, 0.9238795325112867385, 1.000000000000000000),
 ( 0.3333333333333333703, 0.3079598441704289313, 0.3333333333333333703, 0.3079598441704289313, 0.3333333333333333703, 0.3079598441704289313, 0.3333333333333333703, 0.3079598441704289313, 0.3333333333333333703, 0.3079598441704289313, 0.3333333333333333703, 0.3079598441704289313, 0.3333333333333333703, 0.3079598441704289313, 0.3333333333333333703, 0.3079598441704289313, 0.3333333333333333703, 0.3079598441704289313, 0.3333333333333333703, 0.3079598441704289313, 0.3333333333333333703, 0.3079598441704289313, 0.3333333333333333703, 0.3079598441704289313, 0.3333333333333333703, 0.3079598441704289313, 0.3333333333333333703, 0.3079598441704289313, 0.3333333333333333703, 0.3079598441704289313, 0.3333333333333333703, 0.3079598441704289313, 0.3333333333333333703, 0.3079598441704289313, 0.3333333333333333703, 0.3079598441704289313, 0.3333333333333333703, 0.3079598441704289313, 0.3333333333333333703, 0.3079598441704289313, 0.3333333333333333703, 0.3079598441704289313, 0.3333333333333333703, 0.3079598441704289313, 0.3333333333333333703, 0.3079598441704289313, 0.3333333333333333703, 0.3079598441704289313, 0.3333333333333333703, 0.3079598441704289313, 0.3333333333333333703, 0.3079598441704289313, 0.3333333333333333703, 0.3079598441704289313, 0.3333333333333333703, 0.3079598441704289313, 0.3333333333333333703, 0.3079598441704289313, 0.3333333333333333703, 0.3079598441704289313, 0.3333333333333333703, 0.3079598441704289313, 0.3333333333333333703, 0.3079598441704289313, 0.3333333333333333703, 0.3079598441704289313, 0.3333333333333333703, 0.3079598441704289313, 0.3333333333333333703, 0.3079598441704289313, 0.3333333333333333703, 0.3079598441704289313, 0.3333333333333333703, 0.3079598441704289313, 0.3333333333333333703, 0.3079598441704289313, 0.3333333333333333703, 0.3079598441704289313, 0.3333333333333333703, 0.3079598441704289313, 0.3333333333333333703, 0.3079598441704289313, 0.3333333333333333703, 0.3079598441704289313, 0.3333333333333333703, 0.3079598441704289313, 0.3333333333333333703, 0.3079598441704289313, 0.3333333333333333703, 0.3079598441704289313, 0.3333333333333333703, 0.3079598441704289313, 0.3333333333333333703, 0.3079598441704289313, 0.3333333333333333703, 0.3079598441704289313, 0.3333333333333333703),
 ( 0.3333333333333333703, 0.3079598441704289313, 0.3333333333333333703, 0.3079598441704289313, 0.3333333333333333703, 0.3079598441704289313, 0.3333333333333333703, 0.3079598441704289313, 0.3333333333333333703, 0.3079598441704289313, 0.3333333333333333703, 0.3079598441704289313, 0.3333333333333333703, 0.3079598441704289313, 0.3333333333333333703, 0.3079598441704289313, 0.3333333333333333703, 0.3079598441704289313, 0.3333333333333333703, 0.3079598441704289313, 0.3333333333333333703, 0.3079598441704289313, 0.3333333333333333703, 0.3079598441704289313, 0.3333333333333333703, 0.3079598441704289313, 0.3333333333333333703, 0.3079598441704289313, 0.3333333333333333703, 0.3079598441704289313, 0.3333333333333333703, 0.3079598441704289313, 0.3333333333333333703, 0.3079598441704289313, 0.3333333333333333703, 0.3079598441704289313, 0.3333333333333333703, 0.3079598441704289313, 0.3333333333333333703, 0.3079598441704289313, 0.3333333333333333703, 0.3079598441704289313, 0.3333333333333333703, 0.3079598441704289313, 0.3333333333333333703, 0.3079598441704289313, 0.3333333333333333703, 0.3079598441704289313, 0.3333333333333333703, 0.3079598441704289313, 0.3333333333333333703, 0.3079598441704289313, 0.3333333333333333703, 0.3079598441704289313, 0.3333333333333333703, 0.3079598441704289313, 0.3333333333333333703, 0.3079598441704289313, 0.3333333333333333703, 0.3079598441704289313, 0.3333333333333333703, 0.3079598441704289313, 0.3333333333333333703, 0.3079598441704289313, 0.3333333333333333703, 0.3079598441704289313, 0.3333333333333333703, 0.3079598441704289313, 0.3333333333333333703, 0.3079598441704289313, 0.3333333333333333703, 0.3079598441704289313, 0.3333333333333333703, 0.3079598441704289313, 0.3333333333333333703, 0.3079598441704289313, 0.3333333333333333703, 0.3079598441704289313, 0.3333333333333333703, 0.3079598441704289313, 0.3333333333333333703, 0.3079598441704289313, 0.3333333333333333703, 0.3079598441704289313, 0.3333333333333333703, 0.3079598441704289313, 0.3333333333333333703, 0.3079598441704289313, 0.3333333333333333703, 0.3079598441704289313, 0.3333333333333333703, 0.3079598441704289313, 0.3333333333333333703, 0.3079598441704289313, 0.3333333333333333703, 0.3079598441704289313, 0.3333333333333333703),
 ( 1.000000000000000000, 0.9238795325112867385, 1.000000000000000000, 0.9238795325112867385, 1.000000000000000000, 0.9238795325112867385, 1.000000000000000000, 0.9238795325112867385, 1.000000000000000000, 0.9238795325112867385, 1.000000000000000000, 0.9238795325112867385, 1.000000000000000000, 0.9238795325112867385, 1.000000000000000000, 0.9238795325112867385, 1.000000000000000000, 0.9238795325112867385, 1.000000000000000000, 0.9238795325112867385, 1.000000000000000000, 0.9238795325112867385, 1.000000000000000000, 0.9238795325112867385, 1.000000000000000000, 0.9238795325112867385, 1.000000000000000000, 0.9238795325112867385, 1.000000000000000000, 0.9238795325112867385, 1.000000000000000000, 0.9238795325112867385, 1.000000000000000000, 0.9238795325112867385, 1.000000000000000000, 0.9238795325112867385, 1.000000000000000000, 0.9238795325112867385, 1.000000000000000000, 0.9238795325112867385, 1.000000000000000000, 0.9238795325112867385, 1.000000000000000000, 0.9238795325112867385, 1.000000000000000000, 0.9238795325112867385, 1.000000000000000000, 0.9238795325112867385, 1.000000000000000000, 0.9238795325112867385, 1.000000000000000000, 0.9238795325112867385, 1.000000000000000000, 0.9238795325112867385, 1.000000000000000000, 0.9238795325112867385, 1.000000000000000000, 0.9238795325112867385, 1.000000000000000000, 0.9238795325112867385, 1.000000000000000000, 0.9238795325112867385, 1.000000000000000000, 0.9238795325112867385, 1.000000000000000000, 0.9238795325112867385, 1.000000000000000000, 0.9238795325112867385, 1.000000000000000000, 0.9238795325112867385, 1.000000000000000000, 0.9238795325112867385, 1.000000000000000000, 0.9238795325112867385, 1.000000000000000000, 0.9238795325112867385, 1.000000000000000000, 0.9238795325112867385, 1.000000000000000000, 0.9238795325112867385, 1.000000000000000000, 0.9238795325112867385, 1.000000000000000000, 0.9238795325112867385, 1.000000000000000000, 0.9238795325112867385, 1.000000000000000000, 0.9238795325112867385, 1.000000000000000000, 0.9238795325112867385, 1.000000000000000000, 0.9238795325112867385, 1.000000000000000000, 0.9238795325112867385, 1.000000000000000000, 0.9238795325112867385, 1.000000000000000000) ) ) 
 REPRESENTATION_ITEM ( '' )  SURFACE ( )  );
#19778 = DIRECTION ( 'NONE',  ( 0.000000000000000000, 0.000000000000000000, 1.000000000000000000 ) ) ;
#19779 = VERTEX_POINT ( 'NONE', #11092 ) ;
#19780 = AXIS2_PLACEMENT_3D ( 'NONE', #3195, #10541, #14482 ) ;
#19781 = DIRECTION ( 'NONE',  ( 1.000000000000000000, 3.273063162220391312E-16, 0.000000000000000000 ) ) ;
#19782 = EDGE_CURVE ( 'NONE', #701, #23515, #16275, .T. ) ;
#19783 = VERTEX_POINT ( 'NONE', #10809 ) ;
#19784 = LINE ( 'NONE', #14555, #4863 ) ;
#19785 = ORIENTED_EDGE ( 'NONE', *, *, #9977, .F. ) ;
#19786 = CARTESIAN_POINT ( 'NONE',  ( 50.09606816583843880, 11.17458954617364242, 11.97181229448534800 ) ) ;
#19787 = CARTESIAN_POINT ( 'NONE',  ( -67.50000000218494733, 11.76776695296636888, 13.23223304703362579 ) ) ;
#19788 = DIRECTION ( 'NONE',  ( 0.000000000000000000, 0.000000000000000000, -1.000000000000000000 ) ) ;
#19789 = CIRCLE ( 'NONE', #22851, 4.000000000000001776 ) ;
#19790 = CARTESIAN_POINT ( 'NONE',  ( -72.05000000109245661, 12.06698730000000097, 14.99999999999999645 ) ) ;
#19791 = CARTESIAN_POINT ( 'NONE',  ( 1.025207404391860050E-15, 3.458734125000000770, 17.43750000136560274 ) ) ;
#19792 = CARTESIAN_POINT ( 'NONE',  ( 9.920644283265380691E-16, 4.000000000000000000, 9.875000002731196602 ) ) ;
#19793 = CARTESIAN_POINT ( 'NONE',  ( 25.00005080000000035, 0.000000000000000000, 0.000000000000000000 ) ) ;
#19794 = VECTOR ( 'NONE', #17910, 1000.000000000000114 ) ;
#19795 = DIRECTION ( 'NONE',  ( 0.000000000000000000, 0.000000000000000000, -1.000000000000000000 ) ) ;
#19796 = CIRCLE ( 'NONE', #19031, 4.000000000000000000 ) ;
#19797 = CARTESIAN_POINT ( 'NONE',  ( 51.03356816583844591, 11.31069182806492712, 17.97181229448534623 ) ) ;
#19798 = DIRECTION ( 'NONE',  ( -1.000000000000000000, 0.000000000000000000, 0.000000000000000000 ) ) ;
#19799 = CARTESIAN_POINT ( 'NONE',  ( -1.656854249492379250, 4.000000000000000000, 18.93750000273119838 ) ) ;
#19800 = CARTESIAN_POINT ( 'NONE',  ( -68.14999999999999147, 11.03553390593273420, 12.49999999999998934 ) ) ;
#19801 = ORIENTED_EDGE ( 'NONE', *, *, #15530, .F. ) ;
#19802 = CARTESIAN_POINT ( 'NONE',  ( -4.000000000000000000, 0.000000000000000000, 0.000000000000000000 ) ) ;
#19803 = CARTESIAN_POINT ( 'NONE',  ( 2.499999999999999556, 10.82112760146736363, 1.975651141462276161 ) ) ;
#19804 = VERTEX_POINT ( 'NONE', #18081 ) ;
#19805 = CARTESIAN_POINT ( 'NONE',  ( 59.43750000000000711, 10.00000000000000711, 17.99999999999999645 ) ) ;
#19806 = CARTESIAN_POINT ( 'NONE',  ( 4.000000000000000000, 4.898587196589412829E-16, 1.925000002731188209 ) ) ;
#19807 = EDGE_CURVE ( 'NONE', #22748, #21720, #9120, .T. ) ;
#19808 = LINE ( 'NONE', #18138, #1714 ) ;
#19809 = VERTEX_POINT ( 'NONE', #3929 ) ;
#19810 = CARTESIAN_POINT ( 'NONE',  ( -1.656854249492380138, -3.999999999999999112, 19.18750000000001066 ) ) ;
#19811 = ORIENTED_EDGE ( 'NONE', *, *, #4539, .F. ) ;
#19812 = FACE_OUTER_BOUND ( 'NONE', #19283, .T. ) ;
#19813 = FACE_OUTER_BOUND ( 'NONE', #2711, .T. ) ;
#19814 = VERTEX_POINT ( 'NONE', #1897 ) ;
#19815 = CARTESIAN_POINT ( 'NONE',  ( 19.99999999999998934, -9.999999999999964473, -50.00000000000000000 ) ) ;
#19816 =( GEOMETRIC_REPRESENTATION_CONTEXT ( 3 ) GLOBAL_UNCERTAINTY_ASSIGNED_CONTEXT ( ( #11965 ) ) GLOBAL_UNIT_ASSIGNED_CONTEXT ( ( #10127, #10017, #8096 ) ) REPRESENTATION_CONTEXT ( 'NONE', 'WORKASPACE' ) );
#19817 = DIRECTION ( 'NONE',  ( 0.000000000000000000, 0.000000000000000000, -1.000000000000000000 ) ) ;
#19818 = ORIENTED_EDGE ( 'NONE', *, *, #15503, .F. ) ;
#19819 = CARTESIAN_POINT ( 'NONE',  ( -70.60000000218494165, 9.999999999999998224, 12.49999999999999289 ) ) ;
#19820 = CARTESIAN_POINT ( 'NONE',  ( 71.45000000000000284, 12.50000000000000000, 13.96446609406725869 ) ) ;
#19821 = DIRECTION ( 'NONE',  ( 1.000000000000000000, 0.000000000000000000, 0.000000000000000000 ) ) ;
#19822 = AXIS2_PLACEMENT_3D ( 'NONE', #15982, #17888, #10616 ) ;
#19823 = CARTESIAN_POINT ( 'NONE',  ( 57.50231816583843170, 12.78030770151603868, 12.12345345202365188 ) ) ;
#19824 = CARTESIAN_POINT ( 'NONE',  ( -1.432654583217640276, 3.458734125000000326, 0.5500000013655963471 ) ) ;
#19825 = CARTESIAN_POINT ( 'NONE',  ( 1.432654583217641164, 3.458734125000000326, 14.12500000136560452 ) ) ;
#19826 = DIRECTION ( 'NONE',  ( -0.3420201433256622181, 0.9396926207859106484, 1.232595164407828100E-31 ) ) ;
#19827 = CARTESIAN_POINT ( 'NONE',  ( -70.35000000218495586, 7.499999999999996447, 16.03553390593273775 ) ) ;
#19828 = ORIENTED_EDGE ( 'NONE', *, *, #3203, .F. ) ;
#19829 = CARTESIAN_POINT ( 'NONE',  ( 4.999999999999999112, 7.360373001730920350, 4.729683950898897926 ) ) ;
#19830 = AXIS2_PLACEMENT_3D ( 'NONE', #17246, #817, #22730 ) ;
#19831 = CARTESIAN_POINT ( 'NONE',  ( 0.000000000000000000, 0.000000000000000000, 0.000000000000000000 ) ) ;
#19832 = DIRECTION ( 'NONE',  ( 0.000000000000000000, 0.000000000000000000, -1.000000000000000000 ) ) ;
#19833 = VERTEX_POINT ( 'NONE', #9240 ) ;
#19834 = ORIENTED_EDGE ( 'NONE', *, *, #8664, .F. ) ;
#19835 = CARTESIAN_POINT ( 'NONE',  ( 35.00000000000000000, -8.499999999999955591, -4.286263797015736496E-15 ) ) ;
#19836 = ORIENTED_EDGE ( 'NONE', *, *, #22823, .F. ) ;
#19837 = CARTESIAN_POINT ( 'NONE',  ( 60.00000000000000711, 12.82842712474617741, 12.17157287525379239 ) ) ;
#19838 = EDGE_LOOP ( 'NONE', ( #21619, #15679, #3158, #2900 ) ) ;
#19839 = CARTESIAN_POINT ( 'NONE',  ( -6.499999999999999112, -1.264206540070615281, -0.05450957050772532037 ) ) ;
#19840 = EDGE_LOOP ( 'NONE', ( #2426, #5176, #16136, #11661 ) ) ;
#19841 = VECTOR ( 'NONE', #19153, 1000.000000000000114 ) ;
#19842 = CARTESIAN_POINT ( 'NONE',  ( 52.68750000000000711, 9.999999999999978684, 10.99999999999999645 ) ) ;
#19843 = CARTESIAN_POINT ( 'NONE',  ( 66.95000000218496439, 11.03553390593273598, 17.50000000000000355 ) ) ;
#19844 = CARTESIAN_POINT ( 'NONE',  ( 4.000000000001088907, 1.658577278524410170, -3.531553309554541720 ) ) ;
#19845 = ADVANCED_FACE ( 'NONE', ( #1662 ), #5387, .F. ) ;
#19846 = CYLINDRICAL_SURFACE ( 'NONE', #21766, 4.000000000000000888 ) ;
#19847 = CIRCLE ( 'NONE', #9556, 11.00000000000000000 ) ;
#19848 = CARTESIAN_POINT ( 'NONE',  ( 34.99999999999999289, 4.500000000000009770, -50.00000000000000711 ) ) ;
#19849 = FACE_OUTER_BOUND ( 'NONE', #6551, .T. ) ;
#19850 = ORIENTED_EDGE ( 'NONE', *, *, #12050, .T. ) ;
#19851 = CARTESIAN_POINT ( 'NONE',  ( 1.971781867644420635E-15, -4.000000000000000000, 18.37500000273119483 ) ) ;
#19852 = DIRECTION ( 'NONE',  ( -1.000000000000000000, 0.000000000000000000, 0.000000000000000000 ) ) ;
#19853 = CARTESIAN_POINT ( 'NONE',  ( 57.90393183416158251, 14.02818770551463956, 13.41119689145323335 ) ) ;
#19854 = CARTESIAN_POINT ( 'NONE',  ( 30.70991776966726405, -11.25000000000000355, 10.00000000000008882 ) ) ;
#19855 = AXIS2_PLACEMENT_3D ( 'NONE', #586, #20815, #9958 ) ;
#19856 = ADVANCED_FACE ( 'NONE', ( #3581 ), #10916, .F. ) ;
#19857 = CARTESIAN_POINT ( 'NONE',  ( 4.999999999999999112, 3.174628368996077477, 8.152713396088774545 ) ) ;
#19858 = LINE ( 'NONE', #12937, #20048 ) ;
#19859 = AXIS2_PLACEMENT_3D ( 'NONE', #1147, #12323, #2712 ) ;
#19860 = DIRECTION ( 'NONE',  ( 0.9413949561959078505, 0.3373062947069098150, 0.000000000000000000 ) ) ;
#19861 = ORIENTED_EDGE ( 'NONE', *, *, #22256, .F. ) ;
#19862 = CYLINDRICAL_SURFACE ( 'NONE', #14682, 4.000000000000000000 ) ;
#19863 = CARTESIAN_POINT ( 'NONE',  ( 54.84375000000000711, 8.757359312880723223, 18.00000000000000711 ) ) ;
#19864 = DIRECTION ( 'NONE',  ( -0.000000000000000000, -0.000000000000000000, 1.000000000000000000 ) ) ;
#19865 = ORIENTED_EDGE ( 'NONE', *, *, #14816, .F. ) ;
#19866 = DIRECTION ( 'NONE',  ( -0.000000000000000000, -0.000000000000000000, 1.000000000000000000 ) ) ;
#19867 = CARTESIAN_POINT ( 'NONE',  ( -3.458734124999999882, -1.432654583217642497, -1.199999998634403431 ) ) ;
#19868 = CARTESIAN_POINT ( 'NONE',  ( -65.95000000109246230, 8.538419263543522320, 16.46158073645647235 ) ) ;
#19869 =( GEOMETRIC_REPRESENTATION_CONTEXT ( 3 ) GLOBAL_UNCERTAINTY_ASSIGNED_CONTEXT ( ( #17221 ) ) GLOBAL_UNIT_ASSIGNED_CONTEXT ( ( #19944, #18624, #11477 ) ) REPRESENTATION_CONTEXT ( 'NONE', 'WORKASPACE' ) );
#19870 = EDGE_LOOP ( 'NONE', ( #17412, #9466, #12275, #3723, #1397, #10432, #6063 ) ) ;
#19871 = CARTESIAN_POINT ( 'NONE',  ( -65.95000000218495018, 12.50000000000000000, 13.96446609406725692 ) ) ;
#19872 = ORIENTED_EDGE ( 'NONE', *, *, #10467, .T. ) ;
#19873 = FACE_BOUND ( 'NONE', #21504, .T. ) ;
#19874 = ADVANCED_BREP_SHAPE_REPRESENTATION ( '', ( #13661, #7318 ), #14589 ) ;
#19875 = CARTESIAN_POINT ( 'NONE',  ( 4.000000000000000888, 1.656854249492381248, 19.56250000000001421 ) ) ;
#19876 = CARTESIAN_POINT ( 'NONE',  ( 4.000000000000000000, 4.898587196589412829E-16, -1.074999997268812679 ) ) ;
#19877 = AXIS2_PLACEMENT_3D ( 'NONE', #14651, #12, #23606 ) ;
#19878 = EDGE_CURVE ( 'NONE', #10792, #3905, #5616, .T. ) ;
#19879 = DIRECTION ( 'NONE',  ( 0.000000000000000000, 0.000000000000000000, 1.000000000000000000 ) ) ;
#19880 = EDGE_CURVE ( 'NONE', #3988, #1063, #17355, .T. ) ;
#19881 = DIRECTION ( 'NONE',  ( 0.000000000000000000, 0.000000000000000000, -1.000000000000000000 ) ) ;
#19882 = VECTOR ( 'NONE', #11741, 1000.000000000000000 ) ;
#19883 = CARTESIAN_POINT ( 'NONE',  ( -68.20000000000000284, 11.76776695296636888, 13.23223304703362579 ) ) ;
#19884 = VECTOR ( 'NONE', #2312, 1000.000000000000000 ) ;
#19885 = DIRECTION ( 'NONE',  ( 0.000000000000000000, 0.000000000000000000, 1.000000000000000000 ) ) ;
#19886 = ADVANCED_FACE ( 'NONE', ( #13533 ), #22481, .T. ) ;
#19887 = CARTESIAN_POINT ( 'NONE',  ( 59.99999999999997868, 10.93287452463206577, 18.30488221186498521 ) ) ;
#19888 = DIRECTION ( 'NONE',  ( -0.000000000000000000, -1.000000000000000000, -0.000000000000000000 ) ) ;
#19889 = CARTESIAN_POINT ( 'NONE',  ( 4.000000000000000888, -1.656854249492379694, 3.737500000000002931 ) ) ;
#19890 = CARTESIAN_POINT ( 'NONE',  ( -66.25000000109245946, 9.999999999999998224, 12.93301269999999192 ) ) ;
#19891 = CARTESIAN_POINT ( 'NONE',  ( 67.89999999999999147, 7.499999999999996447, 14.99999999999999645 ) ) ;
#19892 = CARTESIAN_POINT ( 'NONE',  ( 1.432654583217641164, 3.458734125000000326, 18.12500000136560274 ) ) ;
#19893 = CARTESIAN_POINT ( 'NONE',  ( -19.99999999999999645, -9.000000000000003553, 5.000000000000079936 ) ) ;
#19894 = ORIENTED_EDGE ( 'NONE', *, *, #4103, .T. ) ;
#19895 = CARTESIAN_POINT ( 'NONE',  ( -7.878064769667250999, -11.25000000000000355, 5.000000000000079936 ) ) ;
#19896 = ORIENTED_EDGE ( 'NONE', *, *, #3099, .T. ) ;
#19897 = CARTESIAN_POINT ( 'NONE',  ( 55.09143183416158962, 11.72490539043799984, 11.02818770551463246 ) ) ;
#19898 = CARTESIAN_POINT ( 'NONE',  ( -66.40000000109247935, 10.85617417291294551, 17.06698729999999742 ) ) ;
#19899 = DIRECTION ( 'NONE',  ( 0.000000000000000000, 0.000000000000000000, 1.000000000000000000 ) ) ;
#19900 = CARTESIAN_POINT ( 'NONE',  ( 3.458734125000000326, 4.235727675282971730E-16, -2.762499998634404097 ) ) ;
#19901 = ORIENTED_EDGE ( 'NONE', *, *, #1236, .T. ) ;
#19902 = VECTOR ( 'NONE', #8034, 1000.000000000000000 ) ;
#19903 = EDGE_CURVE ( 'NONE', #7467, #7989, #14921, .T. ) ;
#19904 = VERTEX_POINT ( 'NONE', #5854 ) ;
#19905 = DIRECTION ( 'NONE',  ( 0.000000000000000000, 0.000000000000000000, 1.000000000000000000 ) ) ;
#19906 = CARTESIAN_POINT ( 'NONE',  ( 59.15625000000002132, 7.000000000000003553, 16.24264068711929099 ) ) ;
#19907 = CARTESIAN_POINT ( 'NONE',  ( -65.45000000218496439, 8.964466094067258695, 17.50000000000000355 ) ) ;
#19908 = EDGE_CURVE ( 'NONE', #2402, #11644, #6092, .T. ) ;
#19909 = CARTESIAN_POINT ( 'NONE',  ( -68.55000000109247082, 8.538419263543524096, 13.53841926354352054 ) ) ;
#19910 = CARTESIAN_POINT ( 'NONE',  ( -3.458734124999998105, -1.432654583217642497, 13.75000000136560452 ) ) ;
#19911 = CARTESIAN_POINT ( 'NONE',  ( -3.999999999999998224, -1.656854249492383246, 11.18750000273119660 ) ) ;
#19912 = ADVANCED_FACE ( 'NONE', ( #19137, #4408, #22360, #15342 ), #20912, .T. ) ;
#19913 = CARTESIAN_POINT ( 'NONE',  ( 54.56250000000000711, 6.999999999999997335, 15.00000000000000533 ) ) ;
#19914 = VECTOR ( 'NONE', #11018, 1000.000000000000000 ) ;
#19915 = CARTESIAN_POINT ( 'NONE',  ( 66.90000000000000568, 9.999999999999998224, 17.49999999999999645 ) ) ;
#19916 = EDGE_CURVE ( 'NONE', #10729, #12579, #16999, .T. ) ;
#19917 = CARTESIAN_POINT ( 'NONE',  ( 52.50000000000000711, 12.12132034355963484, 12.87867965644034740 ) ) ;
#19918 = CARTESIAN_POINT ( 'NONE',  ( 3.458734125000001214, -1.432654583217639610, -0.5749999986344027647 ) ) ;
#19919 = CARTESIAN_POINT ( 'NONE',  ( -0.4410157350360267015, -3.437995502366750777, 2.040000000000000480 ) ) ;
#19920 = CARTESIAN_POINT ( 'NONE',  ( -68.20000000000000284, 11.76776695296636888, 13.23223304703362579 ) ) ;
#19921 = ORIENTED_EDGE ( 'NONE', *, *, #14924, .T. ) ;
#19922 = DIRECTION ( 'NONE',  ( 0.9396926207859107594, -0.3420201433256623291, 3.697785493223492838E-32 ) ) ;
#19923 = CARTESIAN_POINT ( 'NONE',  ( 0.000000000000000000, 0.000000000000000000, 0.000000000000000000 ) ) ;
#19924 = VERTEX_POINT ( 'NONE', #9593 ) ;
#19925 = CARTESIAN_POINT ( 'NONE',  ( 56.62500000000000000, 12.12132034355964727, 17.12132034355963484 ) ) ;
#19926 = CARTESIAN_POINT ( 'NONE',  ( -2.449293598294706907E-16, 4.000000000000000000, -2.824999997268812457 ) ) ;
#19927 = CARTESIAN_POINT ( 'NONE',  ( -27.50000000000000711, 7.500000000000001776, -36.31025403784445871 ) ) ;
#19928 = ORIENTED_EDGE ( 'NONE', *, *, #4797, .T. ) ;
#19929 = CARTESIAN_POINT ( 'NONE',  ( -3.999999999999999112, 0.000000000000000000, 19.00000000000001066 ) ) ;
#19930 = ORIENTED_EDGE ( 'NONE', *, *, #21164, .T. ) ;
#19931 = CARTESIAN_POINT ( 'NONE',  ( 0.000000000000000000, 0.000000000000000000, 0.000000000000000000 ) ) ;
#19932 = DIRECTION ( 'NONE',  ( -1.000000000000000000, -7.703719777548943412E-32, 0.000000000000000000 ) ) ;
#19933 = ORIENTED_EDGE ( 'NONE', *, *, #12290, .T. ) ;
#19934 =( NAMED_UNIT ( * ) SI_UNIT ( $, .STERADIAN. ) SOLID_ANGLE_UNIT ( ) );
#19935 = DIRECTION ( 'NONE',  ( -1.000000000000000000, 0.000000000000000000, 0.000000000000000000 ) ) ;
#19936 = DIRECTION ( 'NONE',  ( 1.000000000000000000, 0.000000000000000000, 0.000000000000000000 ) ) ;
#19937 = CARTESIAN_POINT ( 'NONE',  ( 70.34999999999999432, 7.499999999999995559, 13.96446609406725692 ) ) ;
#19938 = EDGE_CURVE ( 'NONE', #4847, #4037, #5448, .T. ) ;
#19939 = DIRECTION ( 'NONE',  ( 0.000000000000000000, -0.5877852522924624790, -0.8090169943749553338 ) ) ;
#19940 = EDGE_CURVE ( 'NONE', #4468, #8256, #11631, .T. ) ;
#19941 = CARTESIAN_POINT ( 'NONE',  ( 69.45000000218495018, 8.964466094067256918, 17.49999999999999289 ) ) ;
#19942 = CARTESIAN_POINT ( 'NONE',  ( 56.00231816583843170, 12.78030770151603868, 12.12345345202365188 ) ) ;
#19943 = CARTESIAN_POINT ( 'NONE',  ( 1.432654583217642275, -3.458734124999999437, -0.9499999986344030978 ) ) ;
#19944 =( LENGTH_UNIT ( ) NAMED_UNIT ( * ) SI_UNIT ( .MILLI., .METRE. ) );
#19945 = CARTESIAN_POINT ( 'NONE',  ( -1.432654583217639610, -3.458734124999999882, 12.62500000136560629 ) ) ;
#19946 = DIRECTION ( 'NONE',  ( -1.000000000000000000, -7.703719777548943412E-32, 0.000000000000000000 ) ) ;
#19947 = CYLINDRICAL_SURFACE ( 'NONE', #2123, 11.00000000000000000 ) ;
#19948 = VERTEX_POINT ( 'NONE', #11385 ) ;
#19949 = CARTESIAN_POINT ( 'NONE',  ( 45.00000000000000000, -2.399706452296378245, 55.00000000000021316 ) ) ;
#19950 = CARTESIAN_POINT ( 'NONE',  ( 68.29999999999999716, 12.50000000000000000, 14.99999999999999645 ) ) ;
#19951 = PLANE ( 'NONE',  #22695 ) ;
#19952 = ORIENTED_EDGE ( 'NONE', *, *, #241, .T. ) ;
#19953 = VERTEX_POINT ( 'NONE', #2601 ) ;
#19954 = CARTESIAN_POINT ( 'NONE',  ( 2.500000000000000000, 2.357898499370431722, -2.818925648462311528E-15 ) ) ;
#19955 = CARTESIAN_POINT ( 'NONE',  ( 56.15625000000001421, 6.000000000000004441, 16.65685424949239390 ) ) ;
#19956 = VERTEX_POINT ( 'NONE', #20566 ) ;
#19957 = DIRECTION ( 'NONE',  ( -1.000000000000000000, -7.703719777548943412E-32, 0.000000000000000000 ) ) ;
#19958 = VERTEX_POINT ( 'NONE', #18899 ) ;
#19959 = CARTESIAN_POINT ( 'NONE',  ( 51.65625000000000711, 6.000000000000004441, 16.65685424949239390 ) ) ;
#19960 = CARTESIAN_POINT ( 'NONE',  ( 66.50000000218494733, 8.232233047033629347, 13.23223304703362402 ) ) ;
#19961 = DIRECTION ( 'NONE',  ( -1.000000000000000000, -0.000000000000000000, 0.000000000000000000 ) ) ;
#19962 = CARTESIAN_POINT ( 'NONE',  ( -68.89999999999999147, 9.999999999999998224, 12.49999999999999289 ) ) ;
#19963 = DIRECTION ( 'NONE',  ( 0.000000000000000000, 0.000000000000000000, -1.000000000000000000 ) ) ;
#19964 = ORIENTED_EDGE ( 'NONE', *, *, #6308, .T. ) ;
#19965 = CARTESIAN_POINT ( 'NONE',  ( -1.656854249492380138, -3.999999999999999112, 17.31250000273119483 ) ) ;
#19966 = CARTESIAN_POINT ( 'NONE',  ( -2.247776618166720475, 3.308700692843488333, 9.970592379354943802 ) ) ;
#19967 = CARTESIAN_POINT ( 'NONE',  ( 59.31018183416157541, 14.00000000000000000, 15.06805114094561304 ) ) ;
#19968 = CARTESIAN_POINT ( 'NONE',  ( 0.5303295852573085556, -7.199367570657613236, -3.296219944818615577 ) ) ;
#19969 = CARTESIAN_POINT ( 'NONE',  ( 66.55000000109247082, 11.46158073645647235, 16.46158073645647235 ) ) ;
#19970 = CARTESIAN_POINT ( 'NONE',  ( -2.696295709017761055, -5.948846446048906778, 4.997494388800372001E-16 ) ) ;
#19971 = PLANE ( 'NONE',  #22603 ) ;
#19972 = ORIENTED_EDGE ( 'NONE', *, *, #6434, .F. ) ;
#19973 = DIRECTION ( 'NONE',  ( -1.000000000000000000, -7.703719777548943412E-32, 0.000000000000000000 ) ) ;
#19974 = CARTESIAN_POINT ( 'NONE',  ( 58.96875000000000711, 6.999999999999992006, 13.75735931288071967 ) ) ;
#19975 = FACE_OUTER_BOUND ( 'NONE', #22243, .T. ) ;
#19976 = ORIENTED_EDGE ( 'NONE', *, *, #5223, .F. ) ;
#19977 = EDGE_CURVE ( 'NONE', #13567, #15866, #10169, .T. ) ;
#19978 = CARTESIAN_POINT ( 'NONE',  ( -6.170261003233799890, -9.000000000000003553, 5.000000000000079936 ) ) ;
#19979 = CARTESIAN_POINT ( 'NONE',  ( -3.458734125000000326, 1.432654583217640276, -0.3249999986344045411 ) ) ;
#19980 = DIRECTION ( 'NONE',  ( 1.000000000000000000, 7.703719777548943412E-32, 0.000000000000000000 ) ) ;
#19981 = ORIENTED_EDGE ( 'NONE', *, *, #10441, .T. ) ;
#19982 = CARTESIAN_POINT ( 'NONE',  ( 69.99999999999998579, 11.76776695296636888, 16.76776695296636532 ) ) ;
#19983 = EDGE_LOOP ( 'NONE', ( #19921, #11235, #18505, #17362 ) ) ;
#19984 = CARTESIAN_POINT ( 'NONE',  ( -15.00000000000001066, -10.00000000000000000, -49.99999999999999289 ) ) ;
#19985 = CARTESIAN_POINT ( 'NONE',  ( -2.445694354108818303, -2.445694354108820967, 10.81250000136560452 ) ) ;
#19986 = DIRECTION ( 'NONE',  ( -1.000000000000000000, -0.000000000000000000, -0.000000000000000000 ) ) ;
#19987 = CARTESIAN_POINT ( 'NONE',  ( -18.13102059071655248, -8.974600000000002353, 5.000000000000079936 ) ) ;
#19988 = CARTESIAN_POINT ( 'NONE',  ( 19.99999999999998934, 9.999999999999966249, -50.00000000000000000 ) ) ;
#19989 = DIRECTION ( 'NONE',  ( 0.000000000000000000, 0.000000000000000000, -1.000000000000000000 ) ) ;
#19990 = CARTESIAN_POINT ( 'NONE',  ( -68.14999999999999147, 11.03553390593273598, 12.49999999999999289 ) ) ;
#19991 = AXIS2_PLACEMENT_3D ( 'NONE', #18947, #6507, #13827 ) ;
#19992 = DIRECTION ( 'NONE',  ( 0.000000000000000000, 1.224646799147353454E-16, 1.000000000000000000 ) ) ;
#19993 = CARTESIAN_POINT ( 'NONE',  ( -2.445694354108818303, -2.445694354108820523, 17.56250000136560274 ) ) ;
#19994 = CARTESIAN_POINT ( 'NONE',  ( 0.000000000000000000, 6.478011392632982535, -6.807171995660517005 ) ) ;
#19995 = CARTESIAN_POINT ( 'NONE',  ( 3.458734125000000770, 4.235727675282972223E-16, -2.512499998634404097 ) ) ;
#19996 = CARTESIAN_POINT ( 'NONE',  ( 67.84999999999999432, 7.499999999999996447, 16.03553390593273775 ) ) ;
#19997 = CARTESIAN_POINT ( 'NONE',  ( -3.458734124999998993, -1.432654583217642497, 12.50000000136560452 ) ) ;
#19998 = DIRECTION ( 'NONE',  ( -1.000000000000000000, -0.000000000000000000, -0.000000000000000000 ) ) ;
#19999 = ORIENTED_EDGE ( 'NONE', *, *, #22684, .F. ) ;
#20000 = EDGE_CURVE ( 'NONE', #18533, #20897, #2483, .T. ) ;
#20001 = CARTESIAN_POINT ( 'NONE',  ( -68.90000000109247935, 9.143825827087049163, 17.06698730000000097 ) ) ;
#20002 = ORIENTED_EDGE ( 'NONE', *, *, #13932, .T. ) ;
#20003 = CARTESIAN_POINT ( 'NONE',  ( 53.59143183416158962, 11.72490539043799984, 11.02818770551463246 ) ) ;
#20004 = CARTESIAN_POINT ( 'NONE',  ( -67.10000000109248219, 12.06698730000000275, 15.85617417291294196 ) ) ;
#20005 = DIRECTION ( 'NONE',  ( 6.123233995736766036E-17, 1.000000000000000000, 0.000000000000000000 ) ) ;
#20006 = ADVANCED_FACE ( 'NONE', ( #4173 ), #18790, .T. ) ;
#20007 = CARTESIAN_POINT ( 'NONE',  ( 1.656854249492380138, 4.000000000000000000, 1.112500002731187099 ) ) ;
#20008 = VERTEX_POINT ( 'NONE', #4527 ) ;
#20009 = VECTOR ( 'NONE', #12121, 1000.000000000000000 ) ;
#20010 = ORIENTED_EDGE ( 'NONE', *, *, #21776, .T. ) ;
#20011 = DIRECTION ( 'NONE',  ( 1.000000000000000000, 0.000000000000000000, 0.000000000000000000 ) ) ;
#20012 = EDGE_CURVE ( 'NONE', #16796, #12703, #9704, .T. ) ;
#20013 = CARTESIAN_POINT ( 'NONE',  ( 53.28356816583845301, 8.689308171935074654, 12.02818770551464489 ) ) ;
#20014 = CARTESIAN_POINT ( 'NONE',  ( -69.55000000109247082, 11.46158073645647235, 16.46158073645647235 ) ) ;
#20015 = CARTESIAN_POINT ( 'NONE',  ( -68.50000000109245946, 7.933012699999995476, 14.14382582708705094 ) ) ;
#20016 = CARTESIAN_POINT ( 'NONE',  ( 2.445694354108821411, 2.445694354108820523, 12.31250000136560629 ) ) ;
#20017 = CARTESIAN_POINT ( 'NONE',  ( 1.656854249492384135, -3.999999999999999112, 11.43750000273119660 ) ) ;
#20018 = CARTESIAN_POINT ( 'NONE',  ( 55.59375000000000711, 11.24264068711927322, 11.99999999999998934 ) ) ;
#20019 = CARTESIAN_POINT ( 'NONE',  ( 71.95000000000001705, 7.499999999999996447, 13.96446609406725514 ) ) ;
#20020 = CARTESIAN_POINT ( 'NONE',  ( 53.15625000000001421, 7.000000000000003553, 16.24264068711929099 ) ) ;
#20021 = ADVANCED_FACE ( 'NONE', ( #12671 ), #23287, .F. ) ;
#20022 = LINE ( 'NONE', #19562, #18095 ) ;
#20023 = LINE ( 'NONE', #10965, #6875 ) ;
#20024 = ORIENTED_EDGE ( 'NONE', *, *, #14408, .F. ) ;
#20025 = LINE ( 'NONE', #18601, #7553 ) ;
#20026 = DIRECTION ( 'NONE',  ( -0.000000000000000000, -0.000000000000000000, 1.000000000000000000 ) ) ;
#20027 = EDGE_LOOP ( 'NONE', ( #12250, #17629, #19751, #8290, #2000, #1516, #5553, #20033 ) ) ;
#20028 = CARTESIAN_POINT ( 'NONE',  ( 54.09375000000000711, 11.24264068711927322, 11.99999999999998934 ) ) ;
#20029 = APPLICATION_PROTOCOL_DEFINITION ( 'draft international standard', 'automotive_design', 1998, #7335 ) ;
#20030 = CARTESIAN_POINT ( 'NONE',  ( 2.445694354108820523, -2.445694354108820079, 5.112500001365595459 ) ) ;
#20031 = ADVANCED_FACE ( 'NONE', ( #14578 ), #5205, .T. ) ;
#20032 = DIRECTION ( 'NONE',  ( 0.3420201433256622736, 0.9396926207859106484, 0.000000000000000000 ) ) ;
#20033 = ORIENTED_EDGE ( 'NONE', *, *, #13087, .F. ) ;
#20034 = CARTESIAN_POINT ( 'NONE',  ( 1.656854249492381470, 4.000000000000000000, 16.68750000000001066 ) ) ;
#20035 = DIRECTION ( 'NONE',  ( -0.000000000000000000, 0.000000000000000000, 1.000000000000000000 ) ) ;
#20036 = DIRECTION ( 'NONE',  ( 0.3420201433256622736, 0.9396926207859106484, 0.000000000000000000 ) ) ;
#20037 = ORIENTED_EDGE ( 'NONE', *, *, #4702, .T. ) ;
#20038 = ADVANCED_FACE ( 'NONE', ( #8827 ), #3636, .T. ) ;
#20039 = DIRECTION ( 'NONE',  ( 1.000000000000000000, 0.000000000000000000, 0.000000000000000000 ) ) ;
#20040 = ADVANCED_FACE ( 'NONE', ( #13775 ), #21034, .F. ) ;
#20041 = DIRECTION ( 'NONE',  ( 0.000000000000000000, 0.000000000000000000, 1.000000000000000000 ) ) ;
#20042 = CARTESIAN_POINT ( 'NONE',  ( -1.432654583217641164, -3.458734125000000326, 0.1750000013655959863 ) ) ;
#20043 = CARTESIAN_POINT ( 'NONE',  ( 70.09999999999999432, 9.999999999999998224, 17.49999999999999645 ) ) ;
#20044 = CARTESIAN_POINT ( 'NONE',  ( -0.5303295852573156610, 7.199367570657603466, -3.296219944818624903 ) ) ;
#20045 = VECTOR ( 'NONE', #3349, 1000.000000000000114 ) ;
#20046 = DIRECTION ( 'NONE',  ( -7.087422195345011518E-32, -1.000000000000000000, -0.000000000000000000 ) ) ;
#20047 = CARTESIAN_POINT ( 'NONE',  ( 51.87731816583844591, 7.123453452023657206, 12.21969229848395599 ) ) ;
#20048 = VECTOR ( 'NONE', #5252, 1000.000000000000114 ) ;
#20049 = CARTESIAN_POINT ( 'NONE',  ( 3.458734125000000326, 4.235727675282971730E-16, 1.237500001365595903 ) ) ;
#20050 = CARTESIAN_POINT ( 'NONE',  ( 35.28529930323381336, -9.000000000000001776, 5.000000000000079936 ) ) ;
#20051 = CARTESIAN_POINT ( 'NONE',  ( 72.37500000054622262, 9.999999999999998224, 17.28349365000000049 ) ) ;
#20052 = FACE_OUTER_BOUND ( 'NONE', #1380, .T. ) ;
#20053 = ORIENTED_EDGE ( 'NONE', *, *, #16976, .F. ) ;
#20054 = CARTESIAN_POINT ( 'NONE',  ( 65.00000000000000000, 15.00000000000000000, 24.99999999999999645 ) ) ;
#20055 = CARTESIAN_POINT ( 'NONE',  ( 4.688305830332750723, -11.25000000000000355, 5.000000000000079936 ) ) ;
#20056 = ADVANCED_FACE ( 'NONE', ( #17792 ), #15578, .F. ) ;
#20057 = CARTESIAN_POINT ( 'NONE',  ( 67.80000000218494449, 9.999999999999998224, 17.49999999999999645 ) ) ;
#20058 = ORIENTED_EDGE ( 'NONE', *, *, #15381, .F. ) ;
#20059 = EDGE_LOOP ( 'NONE', ( #2431, #23188, #12009, #9376 ) ) ;
#20060 = CARTESIAN_POINT ( 'NONE',  ( 35.00000000000000000, 4.500000000000001776, -20.00000000000000355 ) ) ;
#20061 = EDGE_CURVE ( 'NONE', #11744, #13392, #19808, .T. ) ;
#20062 = VERTEX_POINT ( 'NONE', #10973 ) ;
#20063 = EDGE_CURVE ( 'NONE', #549, #17388, #1718, .T. ) ;
#20064 = CARTESIAN_POINT ( 'NONE',  ( 57.93750000000000000, 10.00000000000001776, 18.99999999999999645 ) ) ;
#20065 = EDGE_LOOP ( 'NONE', ( #7753, #3935, #13947, #9560 ) ) ;
#20066 = LINE ( 'NONE', #12920, #13746 ) ;
#20067 = ORIENTED_EDGE ( 'NONE', *, *, #20605, .T. ) ;
#20068 = EDGE_CURVE ( 'NONE', #23046, #13424, #1363, .T. ) ;
#20069 = CARTESIAN_POINT ( 'NONE',  ( 54.22106816583844591, 14.02818770551465377, 16.58880310854672757 ) ) ;
#20070 = VECTOR ( 'NONE', #21654, 1000.000000000000000 ) ;
#20071 = AXIS2_PLACEMENT_3D ( 'NONE', #4999, #10296, #13765 ) ;
#20072 = CARTESIAN_POINT ( 'NONE',  ( 65.85000000218495586, 11.03553390593273598, 12.49999999999999289 ) ) ;
#20073 = DIRECTION ( 'NONE',  ( -1.000000000000000000, 0.000000000000000000, 0.000000000000000000 ) ) ;
#20074 = DIRECTION ( 'NONE',  ( 1.224646799147353207E-16, 0.000000000000000000, 1.000000000000000000 ) ) ;
#20075 = FACE_OUTER_BOUND ( 'NONE', #11933, .T. ) ;
#20076 = ORIENTED_EDGE ( 'NONE', *, *, #4361, .F. ) ;
#20077 = CARTESIAN_POINT ( 'NONE',  ( -3.999999999999999112, 0.000000000000000000, 17.12500000273119838 ) ) ;
#20078 = DIRECTION ( 'NONE',  ( 1.000000000000000000, -0.000000000000000000, -0.000000000000000000 ) ) ;
#20079 = CARTESIAN_POINT ( 'NONE',  ( 56.40393183416158251, 14.02818770551463956, 13.41119689145323335 ) ) ;
#20080 = CARTESIAN_POINT ( 'NONE',  ( 1.424327985892199999, -3.194194916198549006, 2.040000000000001812 ) ) ;
#20081 = CARTESIAN_POINT ( 'NONE',  ( 65.00000000000000000, -10.00000000000000178, 14.99999999999999467 ) ) ;
#20082 = PLANE ( 'NONE',  #4393 ) ;
#20083 = VECTOR ( 'NONE', #14902, 1000.000000000000114 ) ;
#20084 = DIRECTION ( 'NONE',  ( 0.000000000000000000, 0.000000000000000000, 1.000000000000000000 ) ) ;
#20085 = ORIENTED_EDGE ( 'NONE', *, *, #2914, .T. ) ;
#20086 = FACE_OUTER_BOUND ( 'NONE', #13768, .T. ) ;
#20087 = CARTESIAN_POINT ( 'NONE',  ( 51.93750000000000711, 10.00000000000000711, 17.99999999999999645 ) ) ;
#20088 = LINE ( 'NONE', #9590, #5495 ) ;
#20089 = ORIENTED_EDGE ( 'NONE', *, *, #6663, .F. ) ;
#20090 = CARTESIAN_POINT ( 'NONE',  ( 2.500000000000000444, 0.000000000000000000, -5.000000000000000888 ) ) ;
#20091 = CARTESIAN_POINT ( 'NONE',  ( 1.432654583217642275, -3.458734124999999437, -1.949999998634404319 ) ) ;
#20092 = DIRECTION ( 'NONE',  ( 0.000000000000000000, 0.000000000000000000, -1.000000000000000000 ) ) ;
#20093 = EDGE_CURVE ( 'NONE', #17601, #22004, #16002, .T. ) ;
#20094 = ORIENTED_EDGE ( 'NONE', *, *, #23090, .T. ) ;
#20095 = CARTESIAN_POINT ( 'NONE',  ( 3.999999999999999112, -1.539600717839012978, -3.300726591567080703 ) ) ;
#20096 = ORIENTED_EDGE ( 'NONE', *, *, #21389, .T. ) ;
#20097 = AXIS2_PLACEMENT_3D ( 'NONE', #19482, #16029, #8720 ) ;
#20098 = CARTESIAN_POINT ( 'NONE',  ( -2.413812496766191806, -9.000000000000001776, 5.000000000000079936 ) ) ;
#20099 = CARTESIAN_POINT ( 'NONE',  ( -1.656854249492380138, -3.999999999999999112, 19.18750000000001066 ) ) ;
#20100 = LINE ( 'NONE', #16769, #13819 ) ;
#20101 = DIRECTION ( 'NONE',  ( -0.000000000000000000, 1.000000000000000000, -0.000000000000000000 ) ) ;
#20102 = ORIENTED_EDGE ( 'NONE', *, *, #5551, .T. ) ;
#20103 = LINE ( 'NONE', #3837, #1477 ) ;
#20104 = DIRECTION ( 'NONE',  ( -1.000000000000000000, 0.000000000000000000, 0.000000000000000000 ) ) ;
#20105 = CARTESIAN_POINT ( 'NONE',  ( 66.40000000109247935, 10.85617417291294551, 17.06698729999999742 ) ) ;
#20106 = CARTESIAN_POINT ( 'NONE',  ( 1.025207404391860050E-15, 3.458734125000000326, 16.18750000136560629 ) ) ;
#20107 = CARTESIAN_POINT ( 'NONE',  ( -19.99999999999999645, -9.000000000000003553, 5.000000000000079936 ) ) ;
#20108 =( BOUNDED_CURVE ( )  B_SPLINE_CURVE ( 2, ( #10908, #16629, #14856, #5732, #1769, #93, #3810, #14622, #21882 ),
 .UNSPECIFIED., .F., .F. ) 
 B_SPLINE_CURVE_WITH_KNOTS ( ( 3, 2, 2, 2, 3 ),
 ( 0.000000000000000000, 0.01562499999999990459, 0.03124999999999980918, 0.04687499999999971551, 0.06249999999999961836 ),
 .UNSPECIFIED. ) 
 CURVE ( )  GEOMETRIC_REPRESENTATION_ITEM ( )  RATIONAL_B_SPLINE_CURVE ( ( 1.000000000000000000, 0.9238795325112867385, 1.000000000000000000, 0.9238795325112867385, 1.000000000000000000, 0.9238795325112867385, 1.000000000000000000, 0.9238795325112886259, 0.9999999999999981126 ) ) 
 REPRESENTATION_ITEM ( '' )  );
#20109 = CARTESIAN_POINT ( 'NONE',  ( -3.458734125000000770, 0.000000000000000000, -3.012499998634404541 ) ) ;
#20110 = CARTESIAN_POINT ( 'NONE',  ( 68.40000000218495302, 12.50000000000000000, 14.99999999999999645 ) ) ;
#20111 = CARTESIAN_POINT ( 'NONE',  ( -3.458734124999998993, 1.432654583217640276, 13.37500000136560452 ) ) ;
#20112 = FACE_OUTER_BOUND ( 'NONE', #3503, .T. ) ;
#20113 = VERTEX_POINT ( 'NONE', #8257 ) ;
#20114 = CARTESIAN_POINT ( 'NONE',  ( -68.00000000109247367, 10.85617417291294551, 17.06698730000000097 ) ) ;
#20115 = ORIENTED_EDGE ( 'NONE', *, *, #18490, .T. ) ;
#20116 = CARTESIAN_POINT ( 'NONE',  ( 56.59143183416158962, 11.72490539043799984, 11.02818770551463246 ) ) ;
#20117 = CARTESIAN_POINT ( 'NONE',  ( -72.15000000109246514, 11.46158073645647235, 16.46158073645647235 ) ) ;
#20118 = DIRECTION ( 'NONE',  ( 1.000000000000000000, -6.123233995736766036E-17, -6.123233995736764803E-17 ) ) ;
#20119 = ORIENTED_EDGE ( 'NONE', *, *, #4889, .T. ) ;
#20120 = B_SPLINE_CURVE_WITH_KNOTS ( 'NONE', 3,
 ( #6901, #17795, #21241, #5209, #1246, #4981, #8584, #16355 ),
 .UNSPECIFIED., .F., .F.,
 ( 4, 2, 2, 4 ),
 ( 0.003797433802554436334, 0.004743183970586237024, 0.005688934138618036845, 0.007580434474681636489 ),
 .UNSPECIFIED. ) ;
#20121 = ORIENTED_EDGE ( 'NONE', *, *, #19719, .F. ) ;
#20122 = CARTESIAN_POINT ( 'NONE',  ( -27.50000000000000711, 1.500000000000003109, -33.66025403784446723 ) ) ;
#20123 = CARTESIAN_POINT ( 'NONE',  ( 52.62731816583844591, 12.16943976678978601, 17.07320092032949432 ) ) ;
#20124 = CARTESIAN_POINT ( 'NONE',  ( -71.60000000109246798, 9.143825827087050939, 12.93301269999999370 ) ) ;
#20125 = ADVANCED_FACE ( 'NONE', ( #9059 ), #10550, .T. ) ;
#20126 = AXIS2_PLACEMENT_3D ( 'NONE', #10626, #23516, #12179 ) ;
#20127 = CARTESIAN_POINT ( 'NONE',  ( -69.40000000109246514, 9.143825827087050939, 12.93301269999999370 ) ) ;
#20128 = CARTESIAN_POINT ( 'NONE',  ( -1.432654583217639166, 3.458734125000000770, 12.50000000136560629 ) ) ;
#20129 = CARTESIAN_POINT ( 'NONE',  ( 1.600000000000004086, 0.000000000000000000, -8.073750000000021743 ) ) ;
#20130 = CARTESIAN_POINT ( 'NONE',  ( 51.56250000000000711, 6.999999999999997335, 15.00000000000000533 ) ) ;
#20131 = CARTESIAN_POINT ( 'NONE',  ( 21.00000000000000355, 0.000000000000000000, 0.000000000000000000 ) ) ;
#20132 = CARTESIAN_POINT ( 'NONE',  ( 55.78125000000000000, 8.757359312880703683, 11.99999999999999822 ) ) ;
#20133 = CARTESIAN_POINT ( 'NONE',  ( 4.000000000000000888, 4.898587196589412829E-16, 16.62500000273119838 ) ) ;
#20134 = ADVANCED_FACE ( 'NONE', ( #16235 ), #23646, .T. ) ;
#20135 = CYLINDRICAL_SURFACE ( 'NONE', #364, 6.735000000000022524 ) ;
#20136 = CIRCLE ( 'NONE', #7995, 6.735000000000022524 ) ;
#20137 = TOROIDAL_SURFACE ( 'NONE', #6414, 6.760799999999997034, 0.03079999999999857851 ) ;
#20138 = ORIENTED_EDGE ( 'NONE', *, *, #17898, .F. ) ;
#20139 = DIRECTION ( 'NONE',  ( -1.000000000000000000, 0.000000000000000000, 0.000000000000000000 ) ) ;
#20140 = FACE_OUTER_BOUND ( 'NONE', #16799, .T. ) ;
#20141 = EDGE_LOOP ( 'NONE', ( #5669, #11937, #20216, #18875 ) ) ;
#20142 = CARTESIAN_POINT ( 'NONE',  ( 54.00000000000000711, 12.12132034355963484, 12.87867965644034740 ) ) ;
#20143 =( NAMED_UNIT ( * ) SI_UNIT ( $, .STERADIAN. ) SOLID_ANGLE_UNIT ( ) );
#20144 = CARTESIAN_POINT ( 'NONE',  ( -1.656854249492380804, 4.000000000000000000, -2.762499997268812457 ) ) ;
#20145 = CARTESIAN_POINT ( 'NONE',  ( -60.00000000000001421, -9.999999999999998224, 20.00000000000001421 ) ) ;
#20146 = VERTEX_POINT ( 'NONE', #21475 ) ;
#20147 = CARTESIAN_POINT ( 'NONE',  ( 4.000000000000001776, -1.656854249492379694, 15.43750000000001066 ) ) ;
#20148 = CARTESIAN_POINT ( 'NONE',  ( 4.000000000000000888, -1.656854249492379694, -2.262499999999998401 ) ) ;
#20149 = AXIS2_PLACEMENT_3D ( 'NONE', #10849, #15876, #18125 ) ;
#20150 = CYLINDRICAL_SURFACE ( 'NONE', #9131, 4.000000000000001776 ) ;
#20151 = ORIENTED_EDGE ( 'NONE', *, *, #18231, .F. ) ;
#20152 = LINE ( 'NONE', #5049, #8416 ) ;
#20153 = AXIS2_PLACEMENT_3D ( 'NONE', #12289, #7444, #14758 ) ;
#20154 = CARTESIAN_POINT ( 'NONE',  ( 4.999999999999999112, 6.772677083992387992, 5.538577986808924436 ) ) ;
#20155 = CARTESIAN_POINT ( 'NONE',  ( -3.458734125000000770, 0.000000000000000000, -1.012499998634402543 ) ) ;
#20156 = AXIS2_PLACEMENT_3D ( 'NONE', #18763, #2098, #9436 ) ;
#20157 = VECTOR ( 'NONE', #13748, 1000.000000000000114 ) ;
#20158 = EDGE_CURVE ( 'NONE', #16343, #13221, #14218, .T. ) ;
#20159 = CARTESIAN_POINT ( 'NONE',  ( 69.84999999999999432, 12.50000000000000000, 13.96446609406725869 ) ) ;
#20160 = EDGE_CURVE ( 'NONE', #19948, #18765, #12545, .T. ) ;
#20161 = LINE ( 'NONE', #18264, #13550 ) ;
#20162 = CARTESIAN_POINT ( 'NONE',  ( 2.435583919667260400, -11.25000000000000355, 10.00000000000008882 ) ) ;
#20163 = CARTESIAN_POINT ( 'NONE',  ( 58.90856816583844591, 12.97181229448534978, 13.68930817193506755 ) ) ;
#20164 = CARTESIAN_POINT ( 'NONE',  ( 1.432654583217639832, 3.458734125000000326, -0.5749999986344046521 ) ) ;
#20165 = CARTESIAN_POINT ( 'NONE',  ( 2.445694354108821411, 2.445694354108820523, 16.31250000136560629 ) ) ;
#20166 = EDGE_CURVE ( 'NONE', #19804, #4946, #23524, .T. ) ;
#20167 = DIRECTION ( 'NONE',  ( 1.000000000000000000, 7.703719777548943412E-32, 0.000000000000000000 ) ) ;
#20168 = CARTESIAN_POINT ( 'NONE',  ( 4.999999999999999112, -6.772677083992425295, 5.538577986808878251 ) ) ;
#20169 = ADVANCED_FACE ( 'NONE', ( #3290 ), #10632, .F. ) ;
#20170 = VECTOR ( 'NONE', #3232, 1000.000000000000000 ) ;
#20171 = CARTESIAN_POINT ( 'NONE',  ( -6.989194030332740226, -11.25000000000000355, 5.000000000000079936 ) ) ;
#20172 = VERTEX_POINT ( 'NONE', #4115 ) ;
#20173 = LINE ( 'NONE', #3897, #2674 ) ;
#20174 = LINE ( 'NONE', #3899, #12207 ) ;
#20175 = FACE_OUTER_BOUND ( 'NONE', #20585, .T. ) ;
#20176 = ORIENTED_EDGE ( 'NONE', *, *, #4687, .T. ) ;
#20177 = AXIS2_PLACEMENT_3D ( 'NONE', #20639, #4246, #18965 ) ;
#20178 = ORIENTED_EDGE ( 'NONE', *, *, #8101, .F. ) ;
#20179 = VECTOR ( 'NONE', #6040, 1000.000000000000000 ) ;
#20180 = DIRECTION ( 'NONE',  ( 1.224646799147353207E-16, 0.000000000000000000, 1.000000000000000000 ) ) ;
#20181 = CARTESIAN_POINT ( 'NONE',  ( 53.25000000000000711, 7.171572875253819923, 17.82842712474619873 ) ) ;
#20182 = EDGE_LOOP ( 'NONE', ( #22791, #399 ) ) ;
#20183 = DIRECTION ( 'NONE',  ( 0.000000000000000000, 1.000000000000000000, 0.000000000000000000 ) ) ;
#20184 = VERTEX_POINT ( 'NONE', #162 ) ;
#20185 = CARTESIAN_POINT ( 'NONE',  ( 55.34606816583843880, 8.411196891453267099, 19.02818770551464667 ) ) ;
#20186 = CARTESIAN_POINT ( 'NONE',  ( 70.60000000109246798, 7.933012699999995476, 15.85617417291294196 ) ) ;
#20187 = VECTOR ( 'NONE', #7215, 1000.000000000000000 ) ;
#20188 = DIRECTION ( 'NONE',  ( -0.9021819276639965191, 0.000000000000000000, 0.4313557341643617371 ) ) ;
#20189 = CARTESIAN_POINT ( 'NONE',  ( 72.05000000109245661, 12.06698730000000097, 14.99999999999999645 ) ) ;
#20190 = EDGE_CURVE ( 'NONE', #14136, #16438, #9774, .T. ) ;
#20191 = CARTESIAN_POINT ( 'NONE',  ( -6.500000000000000000, -3.752776749732573247, -3.119443416399232394 ) ) ;
#20192 = ORIENTED_EDGE ( 'NONE', *, *, #10467, .F. ) ;
#20193 = CARTESIAN_POINT ( 'NONE',  ( -2.828427124746188515, -2.828427124746190735, 16.25000000273119838 ) ) ;
#20194 = VECTOR ( 'NONE', #2094, 1000.000000000000000 ) ;
#20195 = CARTESIAN_POINT ( 'NONE',  ( -0.3461262719736137305, 4.658553426539289610, -3.671615880910373608 ) ) ;
#20196 = VECTOR ( 'NONE', #9323, 1000.000000000000000 ) ;
#20197 = CARTESIAN_POINT ( 'NONE',  ( 56.68518183416157541, 10.06805114094561659, 10.99999999999999645 ) ) ;
#20198 = LINE ( 'NONE', #18186, #19914 ) ;
#20199 = EDGE_CURVE ( 'NONE', #18467, #18845, #16289, .T. ) ;
#20200 = CARTESIAN_POINT ( 'NONE',  ( 21.28513981966725765, -11.25000000000000355, 5.000000000000079936 ) ) ;
#20201 = LINE ( 'NONE', #22110, #22344 ) ;
#20202 = EDGE_CURVE ( 'NONE', #2992, #21075, #7382, .T. ) ;
#20203 = CARTESIAN_POINT ( 'NONE',  ( 4.000000000000000000, -2.511475576507276042, -3.469253905236643565 ) ) ;
#20204 = ORIENTED_EDGE ( 'NONE', *, *, #18738, .T. ) ;
#20205 = CARTESIAN_POINT ( 'NONE',  ( -4.000000000000000000, -2.309401076758512694, -5.000000000000000000 ) ) ;
#20206 = CARTESIAN_POINT ( 'NONE',  ( 52.59375000000000711, 11.24264068711927322, 11.99999999999998934 ) ) ;
#20207 = CARTESIAN_POINT ( 'NONE',  ( 4.999999999999999112, -1.699438267350307008, -9.241976615262174732 ) ) ;
#20208 = AXIS2_PLACEMENT_3D ( 'NONE', #17016, #13668, #22502 ) ;
#20209 = ORIENTED_EDGE ( 'NONE', *, *, #4804, .F. ) ;
#20210 = AXIS2_PLACEMENT_3D ( 'NONE', #643, #6048, #13375 ) ;
#20211 = CYLINDRICAL_SURFACE ( 'NONE', #17421, 8.749000000000002331 ) ;
#20212 = CARTESIAN_POINT ( 'NONE',  ( -3.999999999999999112, 0.000000000000000000, 15.12500000273119660 ) ) ;
#20213 = DIRECTION ( 'NONE',  ( -1.000000000000000000, -0.000000000000000000, -0.000000000000000000 ) ) ;
#20214 = LINE ( 'NONE', #3383, #12938 ) ;
#20215 = ORIENTED_EDGE ( 'NONE', *, *, #22970, .F. ) ;
#20216 = ORIENTED_EDGE ( 'NONE', *, *, #4730, .F. ) ;
#20217 = DIRECTION ( 'NONE',  ( 0.000000000000000000, 0.000000000000000000, 1.000000000000000000 ) ) ;
#20218 = VECTOR ( 'NONE', #9923, 1000.000000000000000 ) ;
#20219 = CARTESIAN_POINT ( 'NONE',  ( -3.999999999999999112, 1.656854249492380804, 13.93750000000001243 ) ) ;
#20220 = DIRECTION ( 'NONE',  ( 0.000000000000000000, 0.000000000000000000, -1.000000000000000000 ) ) ;
#20221 = CIRCLE ( 'NONE', #9938, 2.500000000000002220 ) ;
#20222 = CARTESIAN_POINT ( 'NONE',  ( -12.79329400524661331, -6.376973530802017898, 10.00000000000008882 ) ) ;
#20223 = DIRECTION ( 'NONE',  ( 1.224646799147353207E-16, 0.000000000000000000, 1.000000000000000000 ) ) ;
#20224 = AXIS2_PLACEMENT_3D ( 'NONE', #16898, #13547, #473 ) ;
#20225 = VERTEX_POINT ( 'NONE', #18487 ) ;
#20226 = VECTOR ( 'NONE', #20464, 1000.000000000000000 ) ;
#20227 = CARTESIAN_POINT ( 'NONE',  ( -66.84999999999999432, 11.03553390593273598, 17.50000000000000355 ) ) ;
#20228 = DIRECTION ( 'NONE',  ( 1.000000000000000000, 0.000000000000000000, 0.000000000000000000 ) ) ;
#20229 = EDGE_CURVE ( 'NONE', #10792, #18482, #22424, .T. ) ;
#20230 = CARTESIAN_POINT ( 'NONE',  ( 67.65000000109247935, 9.999999999999998224, 12.93301269999999192 ) ) ;
#20231 = CARTESIAN_POINT ( 'NONE',  ( -1.432654583217639610, -3.458734124999999882, 17.62500000136560274 ) ) ;
#20232 = CARTESIAN_POINT ( 'NONE',  ( -6.473970235329672780E-16, -4.862606272033106691, -3.745885042887442395 ) ) ;
#20233 = EDGE_CURVE ( 'NONE', #23046, #433, #7907, .T. ) ;
#20234 = ADVANCED_FACE ( 'NONE', ( #276 ), #2502, .T. ) ;
#20235 =( GEOMETRIC_REPRESENTATION_CONTEXT ( 3 ) GLOBAL_UNCERTAINTY_ASSIGNED_CONTEXT ( ( #13873 ) ) GLOBAL_UNIT_ASSIGNED_CONTEXT ( ( #7380, #18247, #16122 ) ) REPRESENTATION_CONTEXT ( 'NONE', 'WORKASPACE' ) );
#20236 = AXIS2_PLACEMENT_3D ( 'NONE', #8690, #16462, #3157 ) ;
#20237 = CARTESIAN_POINT ( 'NONE',  ( -4.000000000000000000, -1.656854249492383246, 5.362500000000002487 ) ) ;
#20238 = DIRECTION ( 'NONE',  ( -0.9396926207859107594, -0.3420201433256623291, 1.540743955509804830E-32 ) ) ;
#20239 = CARTESIAN_POINT ( 'NONE',  ( 3.458734125000002102, -1.432654583217639610, 11.87500000136560452 ) ) ;
#20240 = DIRECTION ( 'NONE',  ( 0.000000000000000000, 0.000000000000000000, 1.000000000000000000 ) ) ;
#20241 = ORIENTED_EDGE ( 'NONE', *, *, #15381, .T. ) ;
#20242 = CARTESIAN_POINT ( 'NONE',  ( -68.25000000109247367, 7.933012699999995476, 14.99999999999999645 ) ) ;
#20243 = EDGE_LOOP ( 'NONE', ( #726, #11809, #1520, #17035 ) ) ;
#20244 = CARTESIAN_POINT ( 'NONE',  ( 55.37268183416157541, 7.219692298483935566, 12.12345345202367675 ) ) ;
#20245 = CARTESIAN_POINT ( 'NONE',  ( -71.65000000109246514, 7.933012699999995476, 14.99999999999999645 ) ) ;
#20246 = CONTEXT_DEPENDENT_SHAPE_REPRESENTATION ( #6406, #321 ) ;
#20247 = CONICAL_SURFACE ( 'NONE', #6880, 6.500000000000000888, 1.047197551196596521 ) ;
#20248 = CARTESIAN_POINT ( 'NONE',  ( -3.999999999999999112, 0.000000000000000000, 17.00000000000001066 ) ) ;
#20249 = ORIENTED_EDGE ( 'NONE', *, *, #8079, .F. ) ;
#20250 = AXIS2_PLACEMENT_3D ( 'NONE', #4838, #15653, #1562 ) ;
#20251 = ORIENTED_EDGE ( 'NONE', *, *, #8131, .F. ) ;
#20252 = CARTESIAN_POINT ( 'NONE',  ( 71.14999999999999147, 7.499999999999996447, 13.96446609406725514 ) ) ;
#20253 = CARTESIAN_POINT ( 'NONE',  ( 58.12500000000000000, 12.12132034355964727, 17.12132034355963484 ) ) ;
#20254 = CARTESIAN_POINT ( 'NONE',  ( -70.85000000109246798, 9.999999999999998224, 12.93301269999999192 ) ) ;
#20255 = VECTOR ( 'NONE', #22898, 1000.000000000000000 ) ;
#20256 = CARTESIAN_POINT ( 'NONE',  ( -70.95000000109247651, 8.538419263543524096, 13.53841926354352054 ) ) ;
#20257 =( BOUNDED_CURVE ( )  B_SPLINE_CURVE ( 2, ( #18226, #18351, #22159, #1809, #18464, #9157, #22033, #5648, #20248 ),
 .UNSPECIFIED., .F., .F. ) 
 B_SPLINE_CURVE_WITH_KNOTS ( ( 3, 2, 2, 2, 3 ),
 ( 0.2500000000000000000, 0.2625000000000000111, 0.2750000000000000222, 0.2874999999999999778, 0.2999999999999999889 ),
 .UNSPECIFIED. ) 
 CURVE ( )  GEOMETRIC_REPRESENTATION_ITEM ( )  RATIONAL_B_SPLINE_CURVE ( ( 1.000000000000000000, 0.9238795325112867385, 1.000000000000000000, 0.9238795325112867385, 1.000000000000000000, 0.9238795325112867385, 1.000000000000000000, 0.9238795325112867385, 1.000000000000000000 ) ) 
 REPRESENTATION_ITEM ( '' )  );
#20258 = CARTESIAN_POINT ( 'NONE',  ( 1.432654583217641386, 3.458734125000000770, 13.37500000136560274 ) ) ;
#20259 = CARTESIAN_POINT ( 'NONE',  ( 65.97500000054623115, 9.999999999999998224, 17.28349365000000049 ) ) ;
#20260 = CARTESIAN_POINT ( 'NONE',  ( 60.15393183416158962, 6.971812294485357775, 16.17458954617365663 ) ) ;
#20261 = CARTESIAN_POINT ( 'NONE',  ( 4.000000000000000000, 2.309401076758497151, -5.000000000000000000 ) ) ;
#20262 = CIRCLE ( 'NONE', #16836, 4.000000000000001776 ) ;
#20263 = CARTESIAN_POINT ( 'NONE',  ( 51.37500000000000711, 7.878679656440349177, 12.87867965644035984 ) ) ;
#20264 = CARTESIAN_POINT ( 'NONE',  ( -3.999999999999998224, -1.656854249492383246, 15.18750000273119660 ) ) ;
#20265 = CARTESIAN_POINT ( 'NONE',  ( 68.54999999999998295, 8.964466094067287116, 17.50000000000002487 ) ) ;
#20266 = AXIS2_PLACEMENT_3D ( 'NONE', #14756, #6104, #5627 ) ;
#20267 = ORIENTED_EDGE ( 'NONE', *, *, #22089, .T. ) ;
#20268 = CARTESIAN_POINT ( 'NONE',  ( 69.95000000218493597, 12.50000000000000000, 13.96446609406725692 ) ) ;
#20269 = CARTESIAN_POINT ( 'NONE',  ( -70.50000000000000000, 9.999999999999998224, 12.49999999999999289 ) ) ;
#20270 = EDGE_LOOP ( 'NONE', ( #9149, #7136, #13719 ) ) ;
#20271 = CARTESIAN_POINT ( 'NONE',  ( 51.65625000000000711, 7.000000000000003553, 16.24264068711929099 ) ) ;
#20272 = CIRCLE ( 'NONE', #9596, 4.000000000000001776 ) ;
#20273 = CARTESIAN_POINT ( 'NONE',  ( -2.445694354108820523, 2.445694354108820523, 4.612500001365595459 ) ) ;
#20274 = CARTESIAN_POINT ( 'NONE',  ( 0.000000000000000000, 0.000000000000000000, -6.000000000000000888 ) ) ;
#20275 = VERTEX_POINT ( 'NONE', #20274 ) ;
#20276 = CARTESIAN_POINT ( 'NONE',  ( -3.999999999999998224, -1.656854249492383246, 17.06250000000001421 ) ) ;
#20277 = EDGE_CURVE ( 'NONE', #12317, #9363, #13364, .T. ) ;
#20278 = LINE ( 'NONE', #18252, #21704 ) ;
#20279 = DIRECTION ( 'NONE',  ( 0.9396926207859107594, -0.3420201433256623291, 3.697785493223492838E-32 ) ) ;
#20280 = VERTEX_POINT ( 'NONE', #5801 ) ;
#20281 = B_SPLINE_CURVE_WITH_KNOTS ( 'NONE', 3,
 ( #2975, #11653, #715, #22632, #13911, #4781 ),
 .UNSPECIFIED., .F., .F.,
 ( 4, 2, 4 ),
 ( 0.01049192114530184475, 0.01239128608052813933, 0.01429065101575443392 ),
 .UNSPECIFIED. ) ;
#20282 = CARTESIAN_POINT ( 'NONE',  ( 17.25467643033275067, -11.25000000000000355, 10.00000000000008882 ) ) ;
#20283 = CARTESIAN_POINT ( 'NONE',  ( -2.445694354108820523, 2.445694354108820523, 0.8625000013655955700 ) ) ;
#20284 = VECTOR ( 'NONE', #8519, 1000.000000000000000 ) ;
#20285 = CARTESIAN_POINT ( 'NONE',  ( 69.39999999999999147, 8.232233047033627571, 16.76776695296636532 ) ) ;
#20286 = CARTESIAN_POINT ( 'NONE',  ( 72.50000000000000000, 9.999999999999998224, 14.99999999999999645 ) ) ;
#20287 = CARTESIAN_POINT ( 'NONE',  ( 0.000000000000000000, -4.472189673936844301, 8.264486777890091673 ) ) ;
#20288 = CARTESIAN_POINT ( 'NONE',  ( 50.56481816583844591, 5.999999999999996447, 15.06805114094564502 ) ) ;
#20289 = CARTESIAN_POINT ( 'NONE',  ( -2.445694354108820523, 2.445694354108820523, 0.6125000013655953479 ) ) ;
#20290 = CARTESIAN_POINT ( 'NONE',  ( 1.872352939448454495E-15, -3.458734125000000770, 15.93750000136560629 ) ) ;
#20291 = CYLINDRICAL_SURFACE ( 'NONE', #212, 4.000000000000001776 ) ;
#20292 = ORIENTED_EDGE ( 'NONE', *, *, #12757, .F. ) ;
#20293 = CARTESIAN_POINT ( 'NONE',  ( -20.00000000000001066, 1.500000000000003109, -50.00000000000000000 ) ) ;
#20294 = CARTESIAN_POINT ( 'NONE',  ( 2.499999999999999556, -1.464956435139620039, 10.90201369670498366 ) ) ;
#20295 = LINE ( 'NONE', #5705, #2464 ) ;
#20296 = CIRCLE ( 'NONE', #10024, 4.000000000000001776 ) ;
#20297 = ORIENTED_EDGE ( 'NONE', *, *, #14815, .F. ) ;
#20298 = EDGE_LOOP ( 'NONE', ( #9702, #20836, #54, #21913 ) ) ;
#20299 = EDGE_CURVE ( 'NONE', #21072, #13238, #4809, .T. ) ;
#20300 = SURFACE_STYLE_USAGE ( .BOTH. , #14835 ) ;
#20301 = EDGE_CURVE ( 'NONE', #18634, #2584, #1834, .T. ) ;
#20302 = CARTESIAN_POINT ( 'NONE',  ( 58.78125000000000711, 8.343145750507600766, 11.00000000000000355 ) ) ;
#20303 = ORIENTED_EDGE ( 'NONE', *, *, #20229, .F. ) ;
#20304 = CARTESIAN_POINT ( 'NONE',  ( 5.000000000000000000, 0.000000000000000000, -1.000000000000000000 ) ) ;
#20305 = ORIENTED_EDGE ( 'NONE', *, *, #9792, .T. ) ;
#20306 = CARTESIAN_POINT ( 'NONE',  ( 53.84606816583843880, 8.411196891453267099, 19.02818770551464667 ) ) ;
#20307 = ADVANCED_FACE ( 'NONE', ( #14690 ), #9410, .F. ) ;
#20308 = CARTESIAN_POINT ( 'NONE',  ( 71.30000000109248504, 9.143825827087049163, 17.06698729999999742 ) ) ;
#20309 = DIRECTION ( 'NONE',  ( 0.000000000000000000, 0.000000000000000000, -1.000000000000000000 ) ) ;
#20310 = CARTESIAN_POINT ( 'NONE',  ( 6.499999999999999112, -3.752776749732574135, -3.119443416399232394 ) ) ;
#20311 = ORIENTED_EDGE ( 'NONE', *, *, #20757, .F. ) ;
#20312 = CARTESIAN_POINT ( 'NONE',  ( -3.999999999999999112, -1.132742959800665972, 19.16772943110984428 ) ) ;
#20313 = LINE ( 'NONE', #20554, #23684 ) ;
#20314 = CARTESIAN_POINT ( 'NONE',  ( 56.87268183416158962, 7.219692298483935566, 12.12345345202367675 ) ) ;
#20315 = CARTESIAN_POINT ( 'NONE',  ( 2.486305999565482150, -2.591796431245380727, 2.040000000000000480 ) ) ;
#20316 = FACE_BOUND ( 'NONE', #7253, .T. ) ;
#20317 = CARTESIAN_POINT ( 'NONE',  ( -2.149474931388144050, -6.264553569211847694, -0.05533025579362477187 ) ) ;
#20318 = CARTESIAN_POINT ( 'NONE',  ( -67.45000000109246230, 9.999999999999998224, 17.06698730000000097 ) ) ;
#20319 = CARTESIAN_POINT ( 'NONE',  ( -0.5303295852573153280, 7.199367570657603466, -0.4037800551813762739 ) ) ;
#20320 = EDGE_LOOP ( 'NONE', ( #23612, #6609, #16202, #12074 ) ) ;
#20321 = CARTESIAN_POINT ( 'NONE',  ( -19.99999999999999645, -15.00000000000001954, 10.00000000000008882 ) ) ;
#20322 = CARTESIAN_POINT ( 'NONE',  ( 0.000000000000000000, 10.90201369670498721, -1.464956435139581403 ) ) ;
#20323 = EDGE_CURVE ( 'NONE', #844, #7387, #12917, .T. ) ;
#20324 = LINE ( 'NONE', #16634, #2429 ) ;
#20325 = EDGE_LOOP ( 'NONE', ( #1075, #5208 ) ) ;
#20326 = DIRECTION ( 'NONE',  ( 1.000000000000000000, -0.000000000000000000, -0.000000000000000000 ) ) ;
#20327 = DIRECTION ( 'NONE',  ( 0.000000000000000000, 0.000000000000000000, 1.000000000000000000 ) ) ;
#20328 = CARTESIAN_POINT ( 'NONE',  ( 54.99999999999992895, 15.00000000000000000, 1.836970198721037478E-15 ) ) ;
#20329 = EDGE_CURVE ( 'NONE', #1913, #13267, #13610, .T. ) ;
#20330 = CARTESIAN_POINT ( 'NONE',  ( -4.000000000000000888, 1.656854249492380582, -2.762499999999997069 ) ) ;
#20331 = ORIENTED_EDGE ( 'NONE', *, *, #12124, .T. ) ;
#20332 = DIRECTION ( 'NONE',  ( -0.000000000000000000, -1.000000000000000000, -0.000000000000000000 ) ) ;
#20333 = EDGE_LOOP ( 'NONE', ( #15868, #17817, #19632 ) ) ;
#20334 = DIRECTION ( 'NONE',  ( -1.000000000000000000, -7.703719777548943412E-32, 0.000000000000000000 ) ) ;
#20335 = CARTESIAN_POINT ( 'NONE',  ( 9.920644283265380691E-16, 4.000000000000000000, 13.75000000000001066 ) ) ;
#20336 = ADVANCED_FACE ( 'NONE', ( #16700 ), #11090, .F. ) ;
#20337 = CARTESIAN_POINT ( 'NONE',  ( 25.00005080000000035, 0.000000000000000000, 0.000000000000000000 ) ) ;
#20338 = EDGE_CURVE ( 'NONE', #1357, #18995, #6339, .T. ) ;
#20339 = DIRECTION ( 'NONE',  ( -1.000000000000000000, -7.703719777548943412E-32, 0.000000000000000000 ) ) ;
#20340 = CARTESIAN_POINT ( 'NONE',  ( 69.80000000109247082, 10.85617417291294551, 17.06698730000000097 ) ) ;
#20341 = EDGE_LOOP ( 'NONE', ( #16155, #11781, #8098, #7819 ) ) ;
#20342 = LINE ( 'NONE', #11763, #9163 ) ;
#20343 = CIRCLE ( 'NONE', #80, 5.000000000000011546 ) ;
#20344 = DIRECTION ( 'NONE',  ( -1.000000000000000000, -0.000000000000000000, 0.000000000000000000 ) ) ;
#20345 = AXIS2_PLACEMENT_3D ( 'NONE', #12745, #18102, #16084 ) ;
#20346 = CARTESIAN_POINT ( 'NONE',  ( 67.80000000109247082, 12.06698730000000275, 14.14382582708705094 ) ) ;
#20347 = CARTESIAN_POINT ( 'NONE',  ( 2.445694354108821411, 2.445694354108820523, 18.06250000136560274 ) ) ;
#20348 = CARTESIAN_POINT ( 'NONE',  ( 55.00000000000000711, -15.00000000000000000, 10.00000000000000000 ) ) ;
#20349 = CARTESIAN_POINT ( 'NONE',  ( -3.458734125000000770, 1.432654583217640498, -1.074999998634403209 ) ) ;
#20350 = CARTESIAN_POINT ( 'NONE',  ( -4.000000000000000000, 0.000000000000000000, 4.299999999999999822 ) ) ;
#20351 = CARTESIAN_POINT ( 'NONE',  ( 4.999999999999999112, 4.057423117305393845, 8.475820894092990443 ) ) ;
#20352 = CARTESIAN_POINT ( 'NONE',  ( -3.458734124999998993, -1.432654583217642497, 15.50000000136560807 ) ) ;
#20353 = FACE_OUTER_BOUND ( 'NONE', #23441, .T. ) ;
#20354 = ORIENTED_EDGE ( 'NONE', *, *, #14924, .F. ) ;
#20355 = CARTESIAN_POINT ( 'NONE',  ( -67.90000000109247935, 12.06698729999999919, 15.85617417291294196 ) ) ;
#20356 = ORIENTED_EDGE ( 'NONE', *, *, #3635, .T. ) ;
#20357 = CARTESIAN_POINT ( 'NONE',  ( 57.00000000000000000, 12.82842712474617741, 12.17157287525379239 ) ) ;
#20358 = CARTESIAN_POINT ( 'NONE',  ( -69.40000000109246514, 9.143825827087050939, 12.93301269999999370 ) ) ;
#20359 = ORIENTED_EDGE ( 'NONE', *, *, #17861, .F. ) ;
#20360 = FACE_OUTER_BOUND ( 'NONE', #18408, .T. ) ;
#20361 = ORIENTED_EDGE ( 'NONE', *, *, #18879, .T. ) ;
#20362 = ADVANCED_FACE ( 'NONE', ( #22058 ), #15165, .T. ) ;
#20363 = VERTEX_POINT ( 'NONE', #3996 ) ;
#20364 = CARTESIAN_POINT ( 'NONE',  ( -3.458734124999999437, 0.000000000000000000, 17.68750000136560274 ) ) ;
#20365 = EDGE_CURVE ( 'NONE', #5980, #5642, #22378, .T. ) ;
#20366 = VECTOR ( 'NONE', #15127, 1000.000000000000000 ) ;
#20367 = CARTESIAN_POINT ( 'NONE',  ( 53.15625000000001421, 7.000000000000003553, 16.24264068711929099 ) ) ;
#20368 = ADVANCED_FACE ( 'NONE', ( #18960 ), #9761, .T. ) ;
#20369 = CARTESIAN_POINT ( 'NONE',  ( -68.10000000109246798, 9.143825827087049163, 17.06698729999999742 ) ) ;
#20370 = AXIS2_PLACEMENT_3D ( 'NONE', #10707, #17985, #1561 ) ;
#20371 = CARTESIAN_POINT ( 'NONE',  ( 69.20000000109246230, 9.143825827087052716, 12.93301269999999192 ) ) ;
#20372 = CARTESIAN_POINT ( 'NONE',  ( -68.70000000109246230, 10.85617417291294551, 12.93301269999999370 ) ) ;
#20373 = CARTESIAN_POINT ( 'NONE',  ( 66.09999999999999432, 9.999999999999998224, 17.49999999999999645 ) ) ;
#20374 = CARTESIAN_POINT ( 'NONE',  ( 19.99999999999999645, 4.500000000000003553, -50.00000000000000000 ) ) ;
#20375 = CARTESIAN_POINT ( 'NONE',  ( 51.84375000000001421, 8.757359312880723223, 18.00000000000000355 ) ) ;
#20376 = LINE ( 'NONE', #14796, #18665 ) ;
#20377 = CARTESIAN_POINT ( 'NONE',  ( 54.09375000000000711, 11.24264068711927322, 11.99999999999998934 ) ) ;
#20378 = CARTESIAN_POINT ( 'NONE',  ( -2.445694354108818303, -2.445694354108820523, 12.56250000136560629 ) ) ;
#20379 = CARTESIAN_POINT ( 'NONE',  ( -3.999999999999999112, 1.656854249492380804, 15.06250000273119483 ) ) ;
#20380 = CARTESIAN_POINT ( 'NONE',  ( 68.64999999999999147, 7.499999999999996447, 16.03553390593273775 ) ) ;
#20381 = AXIS2_PLACEMENT_3D ( 'NONE', #19095, #17668, #19438 ) ;
#20382 = ORIENTED_EDGE ( 'NONE', *, *, #6137, .F. ) ;
#20383 = CARTESIAN_POINT ( 'NONE',  ( -1.506022603841227436, 0.000000000000000000, 0.000000000000000000 ) ) ;
#20384 = DIRECTION ( 'NONE',  ( 1.000000000000000000, 0.000000000000000000, 0.000000000000000000 ) ) ;
#20385 = EDGE_LOOP ( 'NONE', ( #16059, #20096, #18242, #8979 ) ) ;
#20386 = CARTESIAN_POINT ( 'NONE',  ( 55.21875000000000000, 13.00000000000000711, 16.24264068711927322 ) ) ;
#20387 = CARTESIAN_POINT ( 'NONE',  ( 2.828427124746190735, -2.828427124746189847, -3.199999997268812901 ) ) ;
#20388 = VECTOR ( 'NONE', #10913, 1000.000000000000114 ) ;
#20389 = CARTESIAN_POINT ( 'NONE',  ( 118.3095189484530181, -15.00000000000001954, 10.00000000000008882 ) ) ;
#20390 = VERTEX_POINT ( 'NONE', #13594 ) ;
#20391 = CARTESIAN_POINT ( 'NONE',  ( -1.656854249492379250, 4.000000000000000000, 12.81250000000001066 ) ) ;
#20392 = DIRECTION ( 'NONE',  ( 0.000000000000000000, 0.000000000000000000, -1.000000000000000000 ) ) ;
#20393 = CARTESIAN_POINT ( 'NONE',  ( 1.489200000000000079, 0.000000000000000000, -6.760799999999997034 ) ) ;
#20394 = ORIENTED_EDGE ( 'NONE', *, *, #10101, .T. ) ;
#20395 = PRODUCT_DEFINITION_SHAPE ( 'NONE', 'NONE',  #23710 ) ;
#20396 = CLOSED_SHELL ( 'NONE', ( #9136, #21923, #13344, #16131, #20134, #819, #7166, #14976, #706, #82, #15101, #18551, #19134, #1362, #7349, #23421, #14677, #21093, #10580, #21896, #8761, #21298, #10768, #11931, #16380, #22365, #16684, #2022, #171, #7056, #14539, #11402, #3958, #19281, #19367, #16153, #11748, #6470, #3505, #14704, #23063, #11165, #9832, #781, #14032, #8537, #2162, #2309, #18882, #22057, #14648, #6293, #21098, #1699 ) ) ;
#20397 = CARTESIAN_POINT ( 'NONE',  ( 4.999999999999999112, -1.239665997526951724, 9.314797388894888286 ) ) ;
#20398 =( BOUNDED_CURVE ( )  B_SPLINE_CURVE ( 2, ( #2008, #13183, #14995, #16760, #3930, #9349, #15104, #218, #14866 ),
 .UNSPECIFIED., .F., .F. ) 
 B_SPLINE_CURVE_WITH_KNOTS ( ( 3, 2, 2, 2, 3 ),
 ( 0.2500000000000006661, 0.2656250000000005551, 0.2812500000000004441, 0.2968750000000003886, 0.3125000000000002776 ),
 .UNSPECIFIED. ) 
 CURVE ( )  GEOMETRIC_REPRESENTATION_ITEM ( )  RATIONAL_B_SPLINE_CURVE ( ( 0.9999999999999967804, 0.9238795325112899581, 1.000000000000000000, 0.9238795325112867385, 1.000000000000000000, 0.9238795325112867385, 1.000000000000000000, 0.9238795325112854062, 1.000000000000001332 ) ) 
 REPRESENTATION_ITEM ( '' )  );
#20399 = CARTESIAN_POINT ( 'NONE',  ( 2.445694354108820079, 2.445694354108820523, -0.3874999986344038194 ) ) ;
#20400 = CARTESIAN_POINT ( 'NONE',  ( 68.84999999999999432, 8.964466094067258695, 12.49999999999999289 ) ) ;
#20401 = LINE ( 'NONE', #16596, #12790 ) ;
#20402 = EDGE_CURVE ( 'NONE', #8785, #1632, #9738, .T. ) ;
#20403 = CARTESIAN_POINT ( 'NONE',  ( 9.920644283265380691E-16, 4.000000000000000000, 9.875000002731196602 ) ) ;
#20404 = CARTESIAN_POINT ( 'NONE',  ( 50.09606816583843880, 11.58880310854672935, 10.97181229448534445 ) ) ;
#20405 = CARTESIAN_POINT ( 'NONE',  ( -3.458734125000000326, 1.432654583217640276, -3.324999998634403209 ) ) ;
#20406 = CARTESIAN_POINT ( 'NONE',  ( -2.445694354108818303, -2.445694354108820967, 16.81250000136560629 ) ) ;
#20407 = FACE_OUTER_BOUND ( 'NONE', #18406, .T. ) ;
#20408 = CARTESIAN_POINT ( 'NONE',  ( -71.75000000109247367, 8.538419263543524096, 13.53841926354352054 ) ) ;
#20409 = DIRECTION ( 'NONE',  ( -1.000000000000000000, -0.000000000000000000, -0.000000000000000000 ) ) ;
#20410 = ORIENTED_EDGE ( 'NONE', *, *, #147, .T. ) ;
#20411 = DIRECTION ( 'NONE',  ( 1.000000000000000000, -0.000000000000000000, -0.000000000000000000 ) ) ;
#20412 = FACE_OUTER_BOUND ( 'NONE', #716, .T. ) ;
#20413 = CARTESIAN_POINT ( 'NONE',  ( -69.70000000109246230, 9.143825827087049163, 17.06698729999999742 ) ) ;
#20414 = ORIENTED_EDGE ( 'NONE', *, *, #6310, .T. ) ;
#20415 = ORIENTED_EDGE ( 'NONE', *, *, #18619, .F. ) ;
#20416 = DIRECTION ( 'NONE',  ( 0.000000000000000000, -0.5000000000000013323, -0.8660254037844380415 ) ) ;
#20417 = CARTESIAN_POINT ( 'NONE',  ( 57.18750000000000000, 9.999999999999978684, 10.99999999999999645 ) ) ;
#20418 = ORIENTED_EDGE ( 'NONE', *, *, #10465, .F. ) ;
#20419 = DIRECTION ( 'NONE',  ( -0.000000000000000000, -1.000000000000000000, -0.000000000000000000 ) ) ;
#20420 = VERTEX_POINT ( 'NONE', #15969 ) ;
#20421 = CARTESIAN_POINT ( 'NONE',  ( 52.81481816583844591, 14.00000000000000178, 14.93194885905434610 ) ) ;
#20422 = AXIS2_PLACEMENT_3D ( 'NONE', #11144, #4045, #12823 ) ;
#20423 = CARTESIAN_POINT ( 'NONE',  ( 65.55000000218494449, 7.499999999999995559, 16.03553390593273420 ) ) ;
#20424 = CIRCLE ( 'NONE', #12834, 11.00000000000000000 ) ;
#20425 = CARTESIAN_POINT ( 'NONE',  ( 4.000000000000000888, 4.898587196589412829E-16, 21.31370849898476649 ) ) ;
#20426 = CARTESIAN_POINT ( 'NONE',  ( 70.90000000109245093, 7.933012699999995476, 14.14382582708705094 ) ) ;
#20427 = VECTOR ( 'NONE', #595, 1000.000000000000114 ) ;
#20428 = ORIENTED_EDGE ( 'NONE', *, *, #19191, .T. ) ;
#20429 = CARTESIAN_POINT ( 'NONE',  ( 4.000000000000001776, -1.656854249492379694, 15.56250000273119660 ) ) ;
#20430 =( BOUNDED_CURVE ( )  B_SPLINE_CURVE ( 2, ( #13998, #16149, #21259, #14121, #12213, #19483, #5113, #3082, #17704 ),
 .UNSPECIFIED., .F., .F. ) 
 B_SPLINE_CURVE_WITH_KNOTS ( ( 3, 2, 2, 2, 3 ),
 ( 0.7500000000000000000, 0.7624999999999999556, 0.7750000000000000222, 0.7874999999999999778, 0.8000000000000000444 ),
 .UNSPECIFIED. ) 
 CURVE ( )  GEOMETRIC_REPRESENTATION_ITEM ( )  RATIONAL_B_SPLINE_CURVE ( ( 1.000000000000000000, 0.9238795325112867385, 1.000000000000000000, 0.9238795325112867385, 1.000000000000000000, 0.9238795325112867385, 1.000000000000000000, 0.9238795325112867385, 1.000000000000000000 ) ) 
 REPRESENTATION_ITEM ( '' )  );
#20431 = EDGE_CURVE ( 'NONE', #23005, #17845, #23254, .T. ) ;
#20432 = CARTESIAN_POINT ( 'NONE',  ( 4.999999999999999112, 8.734705317681626724, -0.4999240074894757413 ) ) ;
#20433 = EDGE_CURVE ( 'NONE', #5230, #22394, #4032, .T. ) ;
#20434 = CARTESIAN_POINT ( 'NONE',  ( 52.65393183416158251, 5.971812294485358663, 16.58880310854675599 ) ) ;
#20435 = CARTESIAN_POINT ( 'NONE',  ( -12.00000000000000000, 1.469576158976823947E-15, -3.999999999999998224 ) ) ;
#20436 = PLANE ( 'NONE',  #734 ) ;
#20437 = CARTESIAN_POINT ( 'NONE',  ( -2.059999999999998721, 2.522772406243545965E-16, -0.3080913168122742518 ) ) ;
#20438 = DIRECTION ( 'NONE',  ( -1.000000000000000000, -0.000000000000000000, 0.000000000000000000 ) ) ;
#20439 = DIRECTION ( 'NONE',  ( 0.000000000000000000, 0.000000000000000000, 1.000000000000000000 ) ) ;
#20440 = ORIENTED_EDGE ( 'NONE', *, *, #13406, .F. ) ;
#20441 = CARTESIAN_POINT ( 'NONE',  ( 52.96875000000000000, 6.999999999999992006, 13.75735931288071967 ) ) ;
#20442 = DIRECTION ( 'NONE',  ( 1.000000000000000000, 0.000000000000000000, 0.000000000000000000 ) ) ;
#20443 = EDGE_CURVE ( 'NONE', #19718, #6221, #10606, .T. ) ;
#20444 = CIRCLE ( 'NONE', #4009, 6.200000000000021494 ) ;
#20445 = ORIENTED_EDGE ( 'NONE', *, *, #3105, .F. ) ;
#20446 = CARTESIAN_POINT ( 'NONE',  ( -35.00000000000000711, 7.500000000000001776, -49.99999999999998579 ) ) ;
#20447 = FACE_OUTER_BOUND ( 'NONE', #8245, .T. ) ;
#20448 = DIRECTION ( 'NONE',  ( -1.224646799147353207E-16, 0.000000000000000000, -1.000000000000000000 ) ) ;
#20449 = AXIS2_PLACEMENT_3D ( 'NONE', #463, #2725, #16887 ) ;
#20450 = VECTOR ( 'NONE', #18048, 1000.000000000000000 ) ;
#20451 = DIRECTION ( 'NONE',  ( 0.3420201433256622181, -0.9396926207859107594, 0.000000000000000000 ) ) ;
#20452 = VERTEX_POINT ( 'NONE', #12642 ) ;
#20453 = DIRECTION ( 'NONE',  ( 1.000000000000000000, 0.000000000000000000, 0.000000000000000000 ) ) ;
#20454 = ORIENTED_EDGE ( 'NONE', *, *, #7671, .F. ) ;
#20455 = FACE_OUTER_BOUND ( 'NONE', #16614, .T. ) ;
#20456 = CARTESIAN_POINT ( 'NONE',  ( -1.656854249492379250, 4.000000000000000000, 13.81250000000001066 ) ) ;
#20457 = CARTESIAN_POINT ( 'NONE',  ( -3.803704290982251379, 5.309483803148795644, -3.700000000000004619 ) ) ;
#20458 = FACE_OUTER_BOUND ( 'NONE', #11426, .T. ) ;
#20459 = ADVANCED_BREP_SHAPE_REPRESENTATION ( '', ( #14725, #7318 ), #23252 ) ;
#20460 = CARTESIAN_POINT ( 'NONE',  ( 71.30000000109247082, 12.06698729999999919, 15.85617417291294196 ) ) ;
#20461 = VERTEX_POINT ( 'NONE', #15862 ) ;
#20462 = ADVANCED_FACE ( 'NONE', ( #18113 ), #23135, .T. ) ;
#20463 = AXIS2_PLACEMENT_3D ( 'NONE', #732, #13336, #11780 ) ;
#20464 = DIRECTION ( 'NONE',  ( 0.000000000000000000, 0.000000000000000000, 1.000000000000000000 ) ) ;
#20465 = EDGE_CURVE ( 'NONE', #1297, #10020, #21815, .T. ) ;
#20466 = CARTESIAN_POINT ( 'NONE',  ( 4.000000000000000888, 4.898587196589412829E-16, 11.62500000273119660 ) ) ;
#20467 = CARTESIAN_POINT ( 'NONE',  ( 71.65000000109246514, 7.933012699999995476, 14.99999999999999645 ) ) ;
#20468 = CARTESIAN_POINT ( 'NONE',  ( 1.872352939448454495E-15, -3.458734125000000326, 18.68750000136560629 ) ) ;
#20469 = PLANE ( 'NONE',  #15523 ) ;
#20470 = CARTESIAN_POINT ( 'NONE',  ( -2.445694354108820523, 2.445694354108820523, -1.137499998634402765 ) ) ;
#20471 = CARTESIAN_POINT ( 'NONE',  ( -2.828427124746190291, 2.828427124746190291, 0.1750000000000015432 ) ) ;
#20472 = CARTESIAN_POINT ( 'NONE',  ( -71.10000000218494165, 8.232233047033627571, 16.76776695296636532 ) ) ;
#20473 = CARTESIAN_POINT ( 'NONE',  ( 2.445694354108821411, 2.445694354108820523, 15.06250000136560452 ) ) ;
#20474 = CARTESIAN_POINT ( 'NONE',  ( -67.00000000218494733, 9.999999999999998224, 17.49999999999999645 ) ) ;
#20475 = EDGE_CURVE ( 'NONE', #18765, #15228, #19323, .T. ) ;
#20476 = VECTOR ( 'NONE', #11747, 1000.000000000000000 ) ;
#20477 = ADVANCED_FACE ( 'NONE', ( #10367 ), #3139, .T. ) ;
#20478 = CIRCLE ( 'NONE', #13626, 11.00000000000000000 ) ;
#20479 = ORIENTED_EDGE ( 'NONE', *, *, #10277, .F. ) ;
#20480 = CARTESIAN_POINT ( 'NONE',  ( -68.65000000109247935, 12.06698730000000097, 14.99999999999999645 ) ) ;
#20481 = VERTEX_POINT ( 'NONE', #14056 ) ;
#20482 = CARTESIAN_POINT ( 'NONE',  ( 56.62500000000000000, 12.82842712474620228, 17.82842712474617386 ) ) ;
#20483 = CARTESIAN_POINT ( 'NONE',  ( -70.80000000109245661, 7.933012699999995476, 15.85617417291294196 ) ) ;
#20484 = PRODUCT_CONTEXT ( 'NONE', #4859, 'mechanical' ) ;
#20485 = EDGE_LOOP ( 'NONE', ( #21974, #17272, #18245, #10425 ) ) ;
#20486 = CARTESIAN_POINT ( 'NONE',  ( -1.656854249492380582, 4.000000000000000000, 1.237500002731187099 ) ) ;
#20487 = EDGE_LOOP ( 'NONE', ( #12555, #6158, #3079, #19387 ) ) ;
#20488 = AXIS2_PLACEMENT_3D ( 'NONE', #10121, #17414, #17762 ) ;
#20489 = ORIENTED_EDGE ( 'NONE', *, *, #16158, .F. ) ;
#20490 = CARTESIAN_POINT ( 'NONE',  ( 2.445694354108821411, 2.445694354108820523, 15.31250000136560452 ) ) ;
#20491 = CARTESIAN_POINT ( 'NONE',  ( 57.37500000000000000, 7.878679656440349177, 12.87867965644035984 ) ) ;
#20492 = CARTESIAN_POINT ( 'NONE',  ( -67.60000000109248219, 9.143825827087050939, 12.93301269999999370 ) ) ;
#20493 = CARTESIAN_POINT ( 'NONE',  ( 70.70000000109247651, 7.933012699999995476, 14.14382582708705094 ) ) ;
#20494 = CARTESIAN_POINT ( 'NONE',  ( -66.85000000109246798, 7.933012699999995476, 14.99999999999999645 ) ) ;
#20495 = EDGE_CURVE ( 'NONE', #13665, #158, #17057, .T. ) ;
#20496 = DIRECTION ( 'NONE',  ( -7.087422195345011518E-32, -1.000000000000000000, -0.000000000000000000 ) ) ;
#20497 = CARTESIAN_POINT ( 'NONE',  ( 55.56018183416157541, 7.000000000000000000, 14.93194885905437097 ) ) ;
#20498 = CARTESIAN_POINT ( 'NONE',  ( 9.920644283265380691E-16, 4.000000000000000000, 9.875000002731196602 ) ) ;
#20499 = ADVANCED_FACE ( 'NONE', ( #7820 ), #16797, .F. ) ;
#20500 = CARTESIAN_POINT ( 'NONE',  ( -2.117863837641485618E-16, 3.458734125000000770, 5.737500001365596347 ) ) ;
#20501 = CARTESIAN_POINT ( 'NONE',  ( 1.025207404391860050E-15, 3.458734125000000326, 11.18750000136560452 ) ) ;
#20502 = CARTESIAN_POINT ( 'NONE',  ( 2.828427124746192067, -2.828427124746189847, 14.50000000273119660 ) ) ;
#20503 = CARTESIAN_POINT ( 'NONE',  ( 1.025207404391860050E-15, 3.458734125000000770, 10.43750000136560629 ) ) ;
#20504 = ADVANCED_FACE ( 'NONE', ( #5777 ), #7709, .T. ) ;
#20505 = ORIENTED_EDGE ( 'NONE', *, *, #5223, .T. ) ;
#20506 = CARTESIAN_POINT ( 'NONE',  ( -90.00000000000000000, 0.000000000000000000, 0.000000000000000000 ) ) ;
#20507 = ORIENTED_EDGE ( 'NONE', *, *, #18553, .F. ) ;
#20508 = CARTESIAN_POINT ( 'NONE',  ( 56.02893183416158962, 11.17458954617365663, 18.02818770551464311 ) ) ;
#20509 =( LENGTH_UNIT ( ) NAMED_UNIT ( * ) SI_UNIT ( .MILLI., .METRE. ) );
#20510 = CARTESIAN_POINT ( 'NONE',  ( -1.432654583217640276, 3.458734125000000326, 3.550000001365595459 ) ) ;
#20511 = CARTESIAN_POINT ( 'NONE',  ( 2.828427124746189847, 2.828427124746190291, 1.925000000000001377 ) ) ;
#20512 = ORIENTED_EDGE ( 'NONE', *, *, #6174, .T. ) ;
#20513 = CARTESIAN_POINT ( 'NONE',  ( 4.000000000000000888, 1.656854249492381248, 14.56250000000001066 ) ) ;
#20514 = DIRECTION ( 'NONE',  ( -1.000000000000000000, -0.000000000000000000, -0.000000000000000000 ) ) ;
#20515 = FACE_OUTER_BOUND ( 'NONE', #14224, .T. ) ;
#20516 = VERTEX_POINT ( 'NONE', #15025 ) ;
#20517 = AXIS2_PLACEMENT_3D ( 'NONE', #3047, #19922, #10395 ) ;
#20518 = CARTESIAN_POINT ( 'NONE',  ( -71.20000000218495018, 7.499999999999996447, 14.99999999999999645 ) ) ;
#20519 = CARTESIAN_POINT ( 'NONE',  ( 3.458734125000000770, 4.235727675282972223E-16, -0.5124999986344038749 ) ) ;
#20520 = CARTESIAN_POINT ( 'NONE',  ( 69.95000000000000284, 12.50000000000000000, 16.03553390593273420 ) ) ;
#20521 = DIRECTION ( 'NONE',  ( -0.000000000000000000, -0.000000000000000000, -1.000000000000000000 ) ) ;
#20522 = VECTOR ( 'NONE', #964, 1000.000000000000114 ) ;
#20523 = DIRECTION ( 'NONE',  ( -0.000000000000000000, -0.000000000000000000, 1.000000000000000000 ) ) ;
#20524 = CARTESIAN_POINT ( 'NONE',  ( 54.22106816583844591, 14.02818770551465377, 16.58880310854672757 ) ) ;
#20525 = CARTESIAN_POINT ( 'NONE',  ( 3.458734125000001214, -1.432654583217639610, 4.425000001365595459 ) ) ;
#20526 = CARTESIAN_POINT ( 'NONE',  ( 1.432654583217643163, -3.458734124999999882, 16.00000000136560629 ) ) ;
#20527 = ADVANCED_FACE ( 'NONE', ( #11189 ), #5894, .T. ) ;
#20528 = CARTESIAN_POINT ( 'NONE',  ( 68.65000000218495302, 8.964466094067214286, 17.49999999999996092 ) ) ;
#20529 = CARTESIAN_POINT ( 'NONE',  ( -70.50000000109247367, 12.06698729999999919, 15.85617417291294196 ) ) ;
#20530 = AXIS2_PLACEMENT_3D ( 'NONE', #7087, #16076, #16311 ) ;
#20531 = CARTESIAN_POINT ( 'NONE',  ( 1.999999999999998668, 6.200000000000021494, 0.000000000000000000 ) ) ;
#20532 = VERTEX_POINT ( 'NONE', #13218 ) ;
#20533 = LINE ( 'NONE', #17328, #12281 ) ;
#20534 = FACE_OUTER_BOUND ( 'NONE', #18895, .T. ) ;
#20535 = CARTESIAN_POINT ( 'NONE',  ( -70.50000000109247367, 9.143825827087049163, 17.06698729999999742 ) ) ;
#20536 = ORIENTED_EDGE ( 'NONE', *, *, #16539, .F. ) ;
#20537 = ORIENTED_EDGE ( 'NONE', *, *, #1401, .T. ) ;
#20538 = VECTOR ( 'NONE', #16774, 1000.000000000000114 ) ;
#20539 = CARTESIAN_POINT ( 'NONE',  ( -35.00000000000000711, 16.40063509461079150, -43.12916512459903373 ) ) ;
#20540 =( BOUNDED_CURVE ( )  B_SPLINE_CURVE ( 2, ( #22370, #16895, #3826, #7906, #18798, #12839, #3940, #18673, #5981 ),
 .UNSPECIFIED., .F., .F. ) 
 B_SPLINE_CURVE_WITH_KNOTS ( ( 3, 2, 2, 2, 3 ),
 ( 0.4500000000000000111, 0.4625000000000000222, 0.4749999999999999778, 0.4874999999999999889, 0.5000000000000000000 ),
 .UNSPECIFIED. ) 
 CURVE ( )  GEOMETRIC_REPRESENTATION_ITEM ( )  RATIONAL_B_SPLINE_CURVE ( ( 1.000000000000000000, 0.9238795325112867385, 1.000000000000000000, 0.9238795325112867385, 1.000000000000000000, 0.9238795325112867385, 1.000000000000000000, 0.9238795325112867385, 1.000000000000000000 ) ) 
 REPRESENTATION_ITEM ( '' )  );
#20541 = CARTESIAN_POINT ( 'NONE',  ( 52.59375000000000711, 11.65685424949236015, 10.99999999999998579 ) ) ;
#20542 = ORIENTED_EDGE ( 'NONE', *, *, #546, .F. ) ;
#20543 = DIRECTION ( 'NONE',  ( 0.000000000000000000, 0.000000000000000000, 1.000000000000000000 ) ) ;
#20544 = ORIENTED_EDGE ( 'NONE', *, *, #13944, .F. ) ;
#20545 = AXIS2_PLACEMENT_3D ( 'NONE', #4025, #16859, #9319 ) ;
#20546 = AXIS2_PLACEMENT_3D ( 'NONE', #8858, #3443, #13892 ) ;
#20547 = CARTESIAN_POINT ( 'NONE',  ( 52.53356816583844591, 11.72490539043803004, 18.97181229448534268 ) ) ;
#20548 = CARTESIAN_POINT ( 'NONE',  ( 70.30000000109248504, 12.06698730000000275, 15.85617417291294196 ) ) ;
#20549 = CARTESIAN_POINT ( 'NONE',  ( 0.000000000000000000, 1.699438267350372067, 9.241976615262164074 ) ) ;
#20550 = CARTESIAN_POINT ( 'NONE',  ( 43.27628836966725601, -11.25000000000000355, 5.000000000000079936 ) ) ;
#20551 = VERTEX_POINT ( 'NONE', #16558 ) ;
#20552 = CARTESIAN_POINT ( 'NONE',  ( -1.656854249492379250, 4.000000000000000000, 13.93750000273119483 ) ) ;
#20553 = VECTOR ( 'NONE', #22227, 1000.000000000000000 ) ;
#20554 = CARTESIAN_POINT ( 'NONE',  ( -3.999999999999999112, 0.000000000000000000, 19.56250000136560629 ) ) ;
#20555 = CARTESIAN_POINT ( 'NONE',  ( 59.53125000000000000, 11.65685424949239923, 18.99999999999998934 ) ) ;
#20556 = CARTESIAN_POINT ( 'NONE',  ( 4.000000000000001776, -1.656854249492379694, 12.56250000273119838 ) ) ;
#20557 = FACE_OUTER_BOUND ( 'NONE', #6935, .T. ) ;
#20558 = AXIS2_PLACEMENT_3D ( 'NONE', #13369, #15288, #22560 ) ;
#20559 = VECTOR ( 'NONE', #11580, 1000.000000000000000 ) ;
#20560 = CARTESIAN_POINT ( 'NONE',  ( 0.000000000000000000, -1.464956435139469049, -10.90201369670500497 ) ) ;
#20561 = DIRECTION ( 'NONE',  ( 1.000000000000000000, -0.000000000000000000, -0.000000000000000000 ) ) ;
#20562 = ORIENTED_EDGE ( 'NONE', *, *, #7341, .T. ) ;
#20563 = CARTESIAN_POINT ( 'NONE',  ( -4.000000000000000000, -2.512220745329312610, -3.469390707569719901 ) ) ;
#20564 = DIRECTION ( 'NONE',  ( -1.000000000000000000, -7.703719777548943412E-32, 0.000000000000000000 ) ) ;
#20565 = EDGE_LOOP ( 'NONE', ( #17368, #9836, #23643, #16939 ) ) ;
#20566 = CARTESIAN_POINT ( 'NONE',  ( 19.99999999999998934, 4.500000000000003553, -50.00000000000000000 ) ) ;
#20567 = DIRECTION ( 'NONE',  ( -1.000000000000000000, -0.000000000000000000, -0.000000000000000000 ) ) ;
#20568 = CARTESIAN_POINT ( 'NONE',  ( 2.804994570502171047, 3.229033611042449792, -3.526374918436834704 ) ) ;
#20569 = DIRECTION ( 'NONE',  ( -0.000000000000000000, 0.8660254037844392627, 0.4999999999999990008 ) ) ;
#20570 = ORIENTED_EDGE ( 'NONE', *, *, #14039, .F. ) ;
#20571 = CARTESIAN_POINT ( 'NONE',  ( -1.301042606982605321E-15, 7.505553499465137612, -0.5805565836007695601 ) ) ;
#20572 = ORIENTED_EDGE ( 'NONE', *, *, #21051, .F. ) ;
#20573 = VECTOR ( 'NONE', #20575, 1000.000000000000000 ) ;
#20574 = ADVANCED_FACE ( 'NONE', ( #24 ), #15137, .F. ) ;
#20575 = DIRECTION ( 'NONE',  ( 0.000000000000000000, -1.000000000000000000, 0.000000000000000000 ) ) ;
#20576 = CARTESIAN_POINT ( 'NONE',  ( -1.656854249492380138, -3.999999999999999112, 16.18750000000001066 ) ) ;
#20577 = DIRECTION ( 'NONE',  ( -0.3420201433256622181, 0.9396926207859106484, 1.232595164407828100E-31 ) ) ;
#20578 = VECTOR ( 'NONE', #5064, 1000.000000000000000 ) ;
#20579 = AXIS2_PLACEMENT_3D ( 'NONE', #2252, #20567, #7787 ) ;
#20580 = CARTESIAN_POINT ( 'NONE',  ( -1.301042606982605321E-15, 7.505553499465137612, -3.119443416399232394 ) ) ;
#20581 = STYLED_ITEM ( 'NONE', ( #13838 ), #6193 ) ;
#20582 = PLANE ( 'NONE',  #15981 ) ;
#20583 = CARTESIAN_POINT ( 'NONE',  ( 69.50000000109245946, 10.85617417291294551, 12.93301269999999192 ) ) ;
#20584 = EDGE_CURVE ( 'NONE', #21282, #7575, #12864, .T. ) ;
#20585 = EDGE_LOOP ( 'NONE', ( #11578, #23677, #5755, #13005 ) ) ;
#20586 = FACE_OUTER_BOUND ( 'NONE', #17677, .T. ) ;
#20587 = CARTESIAN_POINT ( 'NONE',  ( 4.000000000000000888, 4.898587196589412829E-16, 10.62500000273119660 ) ) ;
#20588 = CARTESIAN_POINT ( 'NONE',  ( 67.40000000109247935, 7.933012699999995476, 15.85617417291294196 ) ) ;
#20589 = CARTESIAN_POINT ( 'NONE',  ( 2.445694354108821411, 2.445694354108820523, 12.06250000136560629 ) ) ;
#20590 = DIRECTION ( 'NONE',  ( -1.000000000000000000, 0.000000000000000000, 1.224646799147353207E-16 ) ) ;
#20591 = AXIS2_PLACEMENT_3D ( 'NONE', #9224, #23690, #3454 ) ;
#20592 = CARTESIAN_POINT ( 'NONE',  ( -3.458734125000000770, 0.000000000000000000, -2.012499998634403653 ) ) ;
#20593 = CARTESIAN_POINT ( 'NONE',  ( 2.828427124746190735, -2.828427124746189847, 2.675000000000002043 ) ) ;
#20594 = CARTESIAN_POINT ( 'NONE',  ( -15.59503895323380362, -9.000000000000003553, 5.000000000000079936 ) ) ;
#20595 = CARTESIAN_POINT ( 'NONE',  ( -3.458734124999998993, 1.432654583217640276, 11.37500000136560452 ) ) ;
#20596 = DIRECTION ( 'NONE',  ( -1.000000000000000000, 0.000000000000000000, -0.000000000000000000 ) ) ;
#20597 = ORIENTED_EDGE ( 'NONE', *, *, #14484, .T. ) ;
#20598 = CARTESIAN_POINT ( 'NONE',  ( -67.15000000109247935, 11.46158073645647235, 16.46158073645647235 ) ) ;
#20599 = VERTEX_POINT ( 'NONE', #11065 ) ;
#20600 = CARTESIAN_POINT ( 'NONE',  ( 56.06250000000000000, 5.999999999999996447, 15.00000000000001599 ) ) ;
#20601 = CARTESIAN_POINT ( 'NONE',  ( -70.60000000109246798, 10.85617417291294551, 17.06698729999999742 ) ) ;
#20602 = ORIENTED_EDGE ( 'NONE', *, *, #17769, .T. ) ;
#20603 = LINE ( 'NONE', #15490, #12498 ) ;
#20604 = EDGE_LOOP ( 'NONE', ( #791, #12985, #11185, #20037 ) ) ;
#20605 = EDGE_CURVE ( 'NONE', #12674, #1126, #9407, .T. ) ;
#20606 = EDGE_CURVE ( 'NONE', #13210, #15511, #6370, .T. ) ;
#20607 = ORIENTED_EDGE ( 'NONE', *, *, #22400, .F. ) ;
#20608 = CARTESIAN_POINT ( 'NONE',  ( -2.445694354108819191, 2.445694354108820523, 18.56250000136560629 ) ) ;
#20609 = CARTESIAN_POINT ( 'NONE',  ( 53.81250000000000711, 13.00000000000000000, 14.99999999999998757 ) ) ;
#20610 = AXIS2_PLACEMENT_3D ( 'NONE', #22599, #9448, #13521 ) ;
#20611 = CARTESIAN_POINT ( 'NONE',  ( -68.35000000109248219, 8.538419263543524096, 13.53841926354352054 ) ) ;
#20612 = SHAPE_REPRESENTATION ( 'motor', ( #7318 ), #13013 ) ;
#20613 = CARTESIAN_POINT ( 'NONE',  ( 67.60000000109248219, 9.143825827087052716, 12.93301269999999192 ) ) ;
#20614 = EDGE_CURVE ( 'NONE', #21869, #735, #12754, .T. ) ;
#20615 = VECTOR ( 'NONE', #2083, 1000.000000000000114 ) ;
#20616 = AXIS2_PLACEMENT_3D ( 'NONE', #8752, #23100, #3222 ) ;
#20617 = CARTESIAN_POINT ( 'NONE',  ( -67.45000000109246230, 9.999999999999998224, 17.06698730000000097 ) ) ;
#20618 = FACE_OUTER_BOUND ( 'NONE', #21256, .T. ) ;
#20619 = CARTESIAN_POINT ( 'NONE',  ( 57.43518183416157541, 9.931948859054372747, 17.99999999999999645 ) ) ;
#20620 = DIRECTION ( 'NONE',  ( 7.087422195345011518E-32, 1.000000000000000000, -0.000000000000000000 ) ) ;
#20621 = CARTESIAN_POINT ( 'NONE',  ( 2.445694354108820967, -2.445694354108820079, 2.362500001365596791 ) ) ;
#20622 = CARTESIAN_POINT ( 'NONE',  ( 1.432654583217641164, 3.458734125000000326, 12.12500000136560629 ) ) ;
#20623 = CARTESIAN_POINT ( 'NONE',  ( 4.000000000000000888, 1.656854249492381248, 16.68750000273119838 ) ) ;
#20624 = FACE_OUTER_BOUND ( 'NONE', #11718, .T. ) ;
#20625 = AXIS2_PLACEMENT_3D ( 'NONE', #9546, #14948, #5933 ) ;
#20626 = ORIENTED_EDGE ( 'NONE', *, *, #6501, .F. ) ;
#20627 = DIRECTION ( 'NONE',  ( -1.000000000000000000, -0.000000000000000000, 0.000000000000000000 ) ) ;
#20628 = ORIENTED_EDGE ( 'NONE', *, *, #12462, .F. ) ;
#20629 = CARTESIAN_POINT ( 'NONE',  ( 57.34143183416159673, 8.689308171935088865, 17.97181229448535689 ) ) ;
#20630 =( NAMED_UNIT ( * ) PLANE_ANGLE_UNIT ( ) SI_UNIT ( $, .RADIAN. ) );
#20631 = CARTESIAN_POINT ( 'NONE',  ( -3.458734125000000326, 0.000000000000000000, 1.737500001365596347 ) ) ;
#20632 = EDGE_CURVE ( 'NONE', #12232, #2705, #20257, .T. ) ;
#20633 = CARTESIAN_POINT ( 'NONE',  ( 16.42649855928345204, -8.974600000000002353, 5.000000000000079936 ) ) ;
#20634 = ORIENTED_EDGE ( 'NONE', *, *, #17317, .F. ) ;
#20635 = CARTESIAN_POINT ( 'NONE',  ( 4.000000000000001776, -1.656854249492379694, 11.43750000000001066 ) ) ;
#20636 = CARTESIAN_POINT ( 'NONE',  ( 4.999999999999999112, 8.152713396088806519, -3.174628368995992655 ) ) ;
#20637 = AXIS2_PLACEMENT_3D ( 'NONE', #12770, #17899, #16116 ) ;
#20638 = EDGE_CURVE ( 'NONE', #2345, #12921, #3854, .T. ) ;
#20639 = CARTESIAN_POINT ( 'NONE',  ( -4.898587196589412829E-16, 0.000000000000000000, -4.000000000000000000 ) ) ;
#20640 = ORIENTED_EDGE ( 'NONE', *, *, #9537, .T. ) ;
#20641 = CARTESIAN_POINT ( 'NONE',  ( -70.65000000218496723, 11.03553390593273598, 12.49999999999999289 ) ) ;
#20642 = EDGE_CURVE ( 'NONE', #18509, #13840, #248, .T. ) ;
#20643 = CARTESIAN_POINT ( 'NONE',  ( 1.236993788156008760E-15, 0.000000000000000000, 21.31370849898476649 ) ) ;
#20644 = VECTOR ( 'NONE', #1467, 1000.000000000000000 ) ;
#20645 = ADVANCED_FACE ( 'NONE', ( #20360 ), #3970, .T. ) ;
#20646 = AXIS2_PLACEMENT_3D ( 'NONE', #22145, #12970, #10824 ) ;
#20647 = CARTESIAN_POINT ( 'NONE',  ( -3.999999999999998224, -1.656854249492383024, 15.06250000000001066 ) ) ;
#20648 = CARTESIAN_POINT ( 'NONE',  ( 67.89999999999999147, 7.499999999999996447, 14.99999999999999645 ) ) ;
#20649 = CARTESIAN_POINT ( 'NONE',  ( -1.656854249492380138, -3.999999999999999112, 11.18750000000000888 ) ) ;
#20650 = AXIS2_PLACEMENT_3D ( 'NONE', #15337, #22718, #8253 ) ;
#20651 = CARTESIAN_POINT ( 'NONE',  ( -67.04999999999999716, 7.499999999999996447, 16.03553390593273775 ) ) ;
#20652 = VECTOR ( 'NONE', #6512, 1000.000000000000000 ) ;
#20653 = CARTESIAN_POINT ( 'NONE',  ( 57.97106816583845301, 6.971812294485350670, 13.82541045382635403 ) ) ;
#20654 = CARTESIAN_POINT ( 'NONE',  ( -2.445694354108820523, 2.445694354108820523, 4.862500001365595459 ) ) ;
#20655 = CARTESIAN_POINT ( 'NONE',  ( -1.432654583217639832, -3.458734125000000326, 16.87500000136560629 ) ) ;
#20656 = CARTESIAN_POINT ( 'NONE',  ( 18.14354716966726144, -11.25000000000000355, 5.000000000000079936 ) ) ;
#20657 = DIRECTION ( 'NONE',  ( 1.000000000000000000, 0.000000000000000000, -4.093947403305266636E-14 ) ) ;
#20658 = CARTESIAN_POINT ( 'NONE',  ( -60.00000000000000711, 9.999999999999998224, 14.99999999999999645 ) ) ;
#20659 = ORIENTED_EDGE ( 'NONE', *, *, #5825, .T. ) ;
#20660 = CARTESIAN_POINT ( 'NONE',  ( -2.725741868435985094, 3.045094352034055429, -3.220599429844047012 ) ) ;
#20661 = CARTESIAN_POINT ( 'NONE',  ( 4.000000000000000888, -1.656854249492379694, 4.862500002731188431 ) ) ;
#20662 = CARTESIAN_POINT ( 'NONE',  ( -69.90000000109247935, 7.933012699999995476, 14.14382582708705094 ) ) ;
#20663 = ORIENTED_EDGE ( 'NONE', *, *, #974, .T. ) ;
#20664 = EDGE_LOOP ( 'NONE', ( #20937, #11432, #3262, #544 ) ) ;
#20665 = DIRECTION ( 'NONE',  ( 1.000000000000000000, 0.000000000000000000, 0.000000000000000000 ) ) ;
#20666 = CARTESIAN_POINT ( 'NONE',  ( 0.000000000000000000, 0.000000000000000000, 9.480888224575631185 ) ) ;
#20667 = EDGE_LOOP ( 'NONE', ( #10401, #3969, #4322, #6962 ) ) ;
#20668 = CYLINDRICAL_SURFACE ( 'NONE', #21373, 11.00000000000000000 ) ;
#20669 = AXIS2_PLACEMENT_3D ( 'NONE', #20337, #18675, #15113 ) ;
#20670 = EDGE_CURVE ( 'NONE', #14446, #15725, #2870, .T. ) ;
#20671 = CARTESIAN_POINT ( 'NONE',  ( 69.10000000109248219, 7.933012699999995476, 14.14382582708705094 ) ) ;
#20672 = EDGE_CURVE ( 'NONE', #21998, #15638, #23538, .T. ) ;
#20673 = CARTESIAN_POINT ( 'NONE',  ( -3.999999999999999112, -1.132742959800665972, 20.04272942837865656 ) ) ;
#20674 = FACE_OUTER_BOUND ( 'NONE', #19838, .T. ) ;
#20675 = ORIENTED_EDGE ( 'NONE', *, *, #6433, .F. ) ;
#20676 = CARTESIAN_POINT ( 'NONE',  ( 1.971781867644420635E-15, -4.000000000000000000, 12.37500000273119838 ) ) ;
#20677 = CARTESIAN_POINT ( 'NONE',  ( 5.000000000000000888, 0.000000000000000000, 0.000000000000000000 ) ) ;
#20678 = CARTESIAN_POINT ( 'NONE',  ( 54.09375000000000711, 11.65685424949236193, 10.99999999999998401 ) ) ;
#20679 = CARTESIAN_POINT ( 'NONE',  ( 1.799999999999999156, 0.000000000000000000, -6.200000000000021494 ) ) ;
#20680 = PLANE ( 'NONE',  #17397 ) ;
#20681 = VECTOR ( 'NONE', #2857, 1000.000000000000000 ) ;
#20682 = DIRECTION ( 'NONE',  ( 1.000000000000000000, 0.000000000000000000, -1.445602896647339163E-16 ) ) ;
#20683 = CARTESIAN_POINT ( 'NONE',  ( -66.95000000109246230, 8.538419263543524096, 13.53841926354352054 ) ) ;
#20684 = EDGE_LOOP ( 'NONE', ( #7408, #5886, #22094, #14117 ) ) ;
#20685 = CYLINDRICAL_SURFACE ( 'NONE', #21393, 2.500000000000002220 ) ;
#20686 = ORIENTED_EDGE ( 'NONE', *, *, #18329, .T. ) ;
#20687 = PLANE ( 'NONE',  #6736 ) ;
#20688 = CARTESIAN_POINT ( 'NONE',  ( 45.00000000000000000, -10.00000000000001599, 34.11836509645782201 ) ) ;
#20689 = ORIENTED_EDGE ( 'NONE', *, *, #10123, .F. ) ;
#20690 = CARTESIAN_POINT ( 'NONE',  ( 69.15000000218495302, 12.50000000000000000, 13.96446609406725692 ) ) ;
#20691 = CARTESIAN_POINT ( 'NONE',  ( -2.828427124746189403, 2.828427124746190291, 15.00000000273119660 ) ) ;
#20692 = CARTESIAN_POINT ( 'NONE',  ( 0.000000000000000000, 0.000000000000000000, 0.000000000000000000 ) ) ;
#20693 = DIRECTION ( 'NONE',  ( -1.000000000000000000, 0.000000000000000000, 0.000000000000000000 ) ) ;
#20694 = ORIENTED_EDGE ( 'NONE', *, *, #23119, .T. ) ;
#20695 = CYLINDRICAL_SURFACE ( 'NONE', #2615, 2.500000000000002220 ) ;
#20696 = ORIENTED_EDGE ( 'NONE', *, *, #3938, .F. ) ;
#20697 = CARTESIAN_POINT ( 'NONE',  ( 2.828427124746191179, 2.828427124746190291, 13.62500000000001066 ) ) ;
#20698 = CARTESIAN_POINT ( 'NONE',  ( -6.500000000000000000, 3.752776749732573247, -3.119443416399232394 ) ) ;
#20699 = ORIENTED_EDGE ( 'NONE', *, *, #9820, .F. ) ;
#20700 = CARTESIAN_POINT ( 'NONE',  ( 19.99999999999998934, 7.500000000000001776, -20.00000000000000000 ) ) ;
#20701 =( LENGTH_UNIT ( ) NAMED_UNIT ( * ) SI_UNIT ( .MILLI., .METRE. ) );
#20702 = CARTESIAN_POINT ( 'NONE',  ( 69.25000000109245946, 7.933012699999995476, 14.99999999999999645 ) ) ;
#20703 = ORIENTED_EDGE ( 'NONE', *, *, #15947, .T. ) ;
#20704 = DIRECTION ( 'NONE',  ( 0.000000000000000000, 0.000000000000000000, 1.000000000000000000 ) ) ;
#20705 = PRODUCT_DEFINITION ( 'UNKNOWN', '', #14535, #10049 ) ;
#20706 = DIRECTION ( 'NONE',  ( 1.000000000000000000, 0.000000000000000000, 0.000000000000000000 ) ) ;
#20707 = CARTESIAN_POINT ( 'NONE',  ( 70.20000000109246230, 9.143825827087050939, 12.93301269999999370 ) ) ;
#20708 = CARTESIAN_POINT ( 'NONE',  ( 1.432654583217641164, 3.458734125000000326, 14.12500000136560452 ) ) ;
#20709 = CARTESIAN_POINT ( 'NONE',  ( 4.999999999999999112, -6.772677083992345359, -5.538577986808975062 ) ) ;
#20710 = ADVANCED_FACE ( 'NONE', ( #8176 ), #1731, .F. ) ;
#20711 = FACE_OUTER_BOUND ( 'NONE', #3580, .T. ) ;
#20712 = CARTESIAN_POINT ( 'NONE',  ( 7.347880794884118750E-16, -4.000000000000000000, -0.4499999999999972911 ) ) ;
#20713 = CARTESIAN_POINT ( 'NONE',  ( -1.656854249492381248, -3.999999999999999112, -3.387499997268812901 ) ) ;
#20714 = CARTESIAN_POINT ( 'NONE',  ( 0.000000000000000000, 0.000000000000000000, 0.000000000000000000 ) ) ;
#20715 = LINE ( 'NONE', #2863, #10337 ) ;
#20716 = ORIENTED_EDGE ( 'NONE', *, *, #20299, .T. ) ;
#20717 = CARTESIAN_POINT ( 'NONE',  ( -65.95000000109247651, 8.538419263543524096, 13.53841926354352054 ) ) ;
#20718 = ORIENTED_EDGE ( 'NONE', *, *, #7871, .T. ) ;
#20719 = CARTESIAN_POINT ( 'NONE',  ( 55.59375000000000711, 11.65685424949236193, 10.99999999999998401 ) ) ;
#20720 = CARTESIAN_POINT ( 'NONE',  ( -67.00000000109247367, 9.143825827087050939, 12.93301269999999370 ) ) ;
#20721 = CONTEXT_DEPENDENT_SHAPE_REPRESENTATION ( #18183, #13371 ) ;
#20722 = VERTEX_POINT ( 'NONE', #4327 ) ;
#20723 = LINE ( 'NONE', #22644, #983 ) ;
#20724 = ORIENTED_EDGE ( 'NONE', *, *, #5858, .F. ) ;
#20725 = ORIENTED_EDGE ( 'NONE', *, *, #6331, .T. ) ;
#20726 = CARTESIAN_POINT ( 'NONE',  ( -3.458734124999999437, 1.432654583217640498, 18.62500000136560274 ) ) ;
#20727 = CARTESIAN_POINT ( 'NONE',  ( 57.00000000000000000, 12.12132034355963484, 12.87867965644034740 ) ) ;
#20728 = CARTESIAN_POINT ( 'NONE',  ( -67.90000000109246514, 12.06698730000000275, 15.85617417291294196 ) ) ;
#20729 = CARTESIAN_POINT ( 'NONE',  ( 70.40000000109249356, 10.85617417291294551, 17.06698730000000097 ) ) ;
#20730 = CARTESIAN_POINT ( 'NONE',  ( -72.20000000000000284, 11.76776695296636888, 13.23223304703362579 ) ) ;
#20731 = DIRECTION ( 'NONE',  ( 1.000000000000000000, 7.703719777548943412E-32, 0.000000000000000000 ) ) ;
#20732 = CARTESIAN_POINT ( 'NONE',  ( 53.87268183416157541, 7.926799079670491466, 12.83056023321021755 ) ) ;
#20733 = LINE ( 'NONE', #15392, #2414 ) ;
#20734 = EDGE_CURVE ( 'NONE', #14420, #14717, #17275, .T. ) ;
#20735 = CARTESIAN_POINT ( 'NONE',  ( -3.458734125000000770, 0.000000000000000000, 2.987500001365597235 ) ) ;
#20736 = EDGE_CURVE ( 'NONE', #6042, #9739, #22711, .T. ) ;
#20737 = CARTESIAN_POINT ( 'NONE',  ( 0.000000000000000000, -5.222868219166784343, -9.680994141368829631 ) ) ;
#20738 = CARTESIAN_POINT ( 'NONE',  ( -3.999999999999998224, -1.656854249492383246, 12.18750000273119838 ) ) ;
#20739 = DIRECTION ( 'NONE',  ( 0.000000000000000000, 0.000000000000000000, 1.000000000000000000 ) ) ;
#20740 = VERTEX_POINT ( 'NONE', #957 ) ;
#20741 = FACE_OUTER_BOUND ( 'NONE', #12303, .T. ) ;
#20742 = ORIENTED_EDGE ( 'NONE', *, *, #12523, .T. ) ;
#20743 = CARTESIAN_POINT ( 'NONE',  ( 56.87268183416158962, 7.926799079670491466, 12.83056023321021755 ) ) ;
#20744 =( NAMED_UNIT ( * ) PLANE_ANGLE_UNIT ( ) SI_UNIT ( $, .RADIAN. ) );
#20745 = CARTESIAN_POINT ( 'NONE',  ( -2.445694354108819635, -2.445694354108820523, 2.862500001365597235 ) ) ;
#20746 = EDGE_CURVE ( 'NONE', #21260, #7327, #18936, .T. ) ;
#20747 = CARTESIAN_POINT ( 'NONE',  ( -2.117863837641485618E-16, 3.458734125000000326, 1.487500001365596125 ) ) ;
#20748 = ORIENTED_EDGE ( 'NONE', *, *, #5092, .T. ) ;
#20749 = CARTESIAN_POINT ( 'NONE',  ( 1.971781867644420635E-15, -4.000000000000000000, 11.25000000000001066 ) ) ;
#20750 = LINE ( 'NONE', #20636, #12960 ) ;
#20751 = CARTESIAN_POINT ( 'NONE',  ( -19.99999999999999645, -9.000000000000003553, 10.00000000000008882 ) ) ;
#20752 = ORIENTED_EDGE ( 'NONE', *, *, #15650, .T. ) ;
#20753 = DIRECTION ( 'NONE',  ( 0.000000000000000000, -1.000000000000000000, 0.000000000000000000 ) ) ;
#20754 = LINE ( 'NONE', #6405, #4872 ) ;
#20755 = CARTESIAN_POINT ( 'NONE',  ( 29.82104703033275328, -11.25000000000000355, 5.000000000000079936 ) ) ;
#20756 = CARTESIAN_POINT ( 'NONE',  ( 3.458734125000002546, -1.432654583217639610, 19.12500000136560629 ) ) ;
#20757 = EDGE_CURVE ( 'NONE', #4629, #2957, #15161, .T. ) ;
#20758 = CARTESIAN_POINT ( 'NONE',  ( 47.24605889071655440, -8.974600000000002353, 5.000000000000079936 ) ) ;
#20759 = CARTESIAN_POINT ( 'NONE',  ( 68.60000000109248219, 12.06698730000000275, 14.14382582708705094 ) ) ;
#20760 = AXIS2_PLACEMENT_3D ( 'NONE', #3341, #18076, #16173 ) ;
#20761 = EDGE_CURVE ( 'NONE', #8065, #15511, #6249, .T. ) ;
#20762 = CARTESIAN_POINT ( 'NONE',  ( 4.999999999999999112, 0.000000000000000000, 0.000000000000000000 ) ) ;
#20763 = CARTESIAN_POINT ( 'NONE',  ( 53.56481816583844591, 6.999999999999998224, 15.06805114094563436 ) ) ;
#20764 = AXIS2_PLACEMENT_3D ( 'NONE', #22772, #1087, #13473 ) ;
#20765 = EDGE_CURVE ( 'NONE', #476, #10312, #10186, .T. ) ;
#20766 = CARTESIAN_POINT ( 'NONE',  ( -2.117863837641485618E-16, 3.458734125000000770, 3.737500001365594571 ) ) ;
#20767 = CARTESIAN_POINT ( 'NONE',  ( -2.445694354108819191, 2.445694354108820523, 12.56250000136560629 ) ) ;
#20768 = CARTESIAN_POINT ( 'NONE',  ( -72.00000000000000000, 8.232233047033629347, 13.23223304703362402 ) ) ;
#20769 = CARTESIAN_POINT ( 'NONE',  ( -70.60000000109246798, 10.85617417291294551, 17.06698730000000097 ) ) ;
#20770 = CARTESIAN_POINT ( 'NONE',  ( 0.000000000000000000, 0.000000000000000000, 0.000000000000000000 ) ) ;
#20771 = DIRECTION ( 'NONE',  ( 0.000000000000000000, 0.000000000000000000, 1.000000000000000000 ) ) ;
#20772 = ORIENTED_EDGE ( 'NONE', *, *, #8180, .F. ) ;
#20773 = CARTESIAN_POINT ( 'NONE',  ( 7.347880794884118750E-16, -4.000000000000000000, 2.675000002731188875 ) ) ;
#20774 = CARTESIAN_POINT ( 'NONE',  ( -69.75000000109247367, 8.538419263543522320, 16.46158073645647235 ) ) ;
#20775 = EDGE_CURVE ( 'NONE', #14210, #9234, #17507, .T. ) ;
#20776 = ORIENTED_EDGE ( 'NONE', *, *, #17717, .F. ) ;
#20777 = EDGE_CURVE ( 'NONE', #18380, #2790, #18189, .T. ) ;
#20778 = VERTEX_POINT ( 'NONE', #610 ) ;
#20779 = CLOSED_SHELL ( 'NONE', ( #14517, #387, #10037, #18282, #9214, #16190, #22222, #9247, #3197, #12487, #19886, #17007, #20336, #19218, #7715, #21316, #20040, #22252, #9597, #1935, #10007, #4979, #7311, #23258, #5804, #20926, #16885, #9421, #1575, #3647, #19642, #10890, #13466, #15234, #20527, #11498, #2037, #16279, #18992, #15826, #19752, #18154, #16949, #3266, #2793, #14611, #9965, #275, #17151, #21832, #11125, #11625, #2955, #11195, #20021, #5129, #20169, #8105, #6577, #13177, #10868, #14008, #18331, #1068, #22703, #15247, #5095, #13018, #13025, #7195, #20056, #10261, #14102, #4673, #7569, #19282, #1302, #3128, #19612, #4575, #18196, #12293, #22404, #20574, #3268, #4064, #8930, #13715, #1707, #7640, #9558, #7923, #19856, #5931, #17833, #17682, #20307, #11046, #22352, #7916, #13491, #14836, #13744, #5270, #18436, #5425, #5619, #4701, #8266, #16354, #7369, #14831, #23302, #879 ) ) ;
#20780 = LINE ( 'NONE', #4384, #22069 ) ;
#20781 = ORIENTED_EDGE ( 'NONE', *, *, #2932, .T. ) ;
#20782 = DIRECTION ( 'NONE',  ( 1.000000000000000000, 7.703719777548943412E-32, 0.000000000000000000 ) ) ;
#20783 = AXIS2_PLACEMENT_3D ( 'NONE', #5690, #23660, #18386 ) ;
#20784 = CARTESIAN_POINT ( 'NONE',  ( 68.90000000109247935, 9.143825827087049163, 17.06698729999999742 ) ) ;
#20785 = CARTESIAN_POINT ( 'NONE',  ( 67.75000000109245946, 8.538419263543524096, 13.53841926354352054 ) ) ;
#20786 = PRODUCT_DEFINITION_SHAPE ( 'NONE', 'NONE',  #10803 ) ;
#20787 = VERTEX_POINT ( 'NONE', #10218 ) ;
#20788 = AXIS2_PLACEMENT_3D ( 'NONE', #21489, #5102, #21371 ) ;
#20789 = LINE ( 'NONE', #18526, #13774 ) ;
#20790 = CARTESIAN_POINT ( 'NONE',  ( 58.96875000000000711, 5.999999999999987566, 13.34314575050763452 ) ) ;
#20791 = EDGE_CURVE ( 'NONE', #4634, #7447, #9985, .T. ) ;
#20792 = DIRECTION ( 'NONE',  ( -1.000000000000000000, 0.000000000000000000, 0.000000000000000000 ) ) ;
#20793 = CARTESIAN_POINT ( 'NONE',  ( 2.445694354108821411, 2.445694354108820523, 19.06250000136560629 ) ) ;
#20794 = CARTESIAN_POINT ( 'NONE',  ( 4.999999999999999112, -4.057423117305452465, 8.475820894092962021 ) ) ;
#20795 = CARTESIAN_POINT ( 'NONE',  ( 50.00000000000000000, 10.00000000000001599, 34.11836509645781490 ) ) ;
#20796 = ORIENTED_EDGE ( 'NONE', *, *, #18195, .F. ) ;
#20797 = LINE ( 'NONE', #4522, #6521 ) ;
#20798 = EDGE_CURVE ( 'NONE', #18765, #7419, #15559, .T. ) ;
#20799 = DIRECTION ( 'NONE',  ( 0.000000000000000000, 0.000000000000000000, 1.000000000000000000 ) ) ;
#20800 = DIRECTION ( 'NONE',  ( 0.000000000000000000, 0.000000000000000000, 1.000000000000000000 ) ) ;
#20801 = EDGE_CURVE ( 'NONE', #1016, #5492, #20603, .T. ) ;
#20802 = ORIENTED_EDGE ( 'NONE', *, *, #17080, .T. ) ;
#20803 = CARTESIAN_POINT ( 'NONE',  ( 4.211140560182196957, 2.431303136016536470, -3.745885042887433514 ) ) ;
#20804 = CARTESIAN_POINT ( 'NONE',  ( -69.40000000218495302, 9.999999999999998224, 17.49999999999999645 ) ) ;
#20805 = CARTESIAN_POINT ( 'NONE',  ( 50.00000000000000000, -10.03966385473554013, 10.00000000000008882 ) ) ;
#20806 = CARTESIAN_POINT ( 'NONE',  ( -1.506022603841227436, 1.012170579495290078E-15, 8.265000000000021885 ) ) ;
#20807 = ORIENTED_EDGE ( 'NONE', *, *, #5590, .F. ) ;
#20808 = FACE_OUTER_BOUND ( 'NONE', #14939, .T. ) ;
#20809 = EDGE_LOOP ( 'NONE', ( #6520, #4167, #20752, #18488, #15778, #1077, #21019, #5560, #16858 ) ) ;
#20810 = CARTESIAN_POINT ( 'NONE',  ( 70.85000000109246798, 9.999999999999998224, 12.93301269999999192 ) ) ;
#20811 = VECTOR ( 'NONE', #9648, 1000.000000000000000 ) ;
#20812 = CARTESIAN_POINT ( 'NONE',  ( -1.656854249492379250, 4.000000000000000000, 10.81250000000001243 ) ) ;
#20813 = CARTESIAN_POINT ( 'NONE',  ( 65.00000000000000000, 9.999999999999998224, 17.49999999999999645 ) ) ;
#20814 = ORIENTED_EDGE ( 'NONE', *, *, #5557, .F. ) ;
#20815 = DIRECTION ( 'NONE',  ( -1.000000000000000000, -7.703719777548943412E-32, 0.000000000000000000 ) ) ;
#20816 = CARTESIAN_POINT ( 'NONE',  ( 70.15000000109246514, 8.538419263543524096, 13.53841926354352054 ) ) ;
#20817 = ORIENTED_EDGE ( 'NONE', *, *, #15801, .F. ) ;
#20818 = DIRECTION ( 'NONE',  ( -1.000000000000000000, -0.000000000000000000, -0.000000000000000000 ) ) ;
#20819 = DIRECTION ( 'NONE',  ( 0.000000000000000000, -0.000000000000000000, -1.000000000000000000 ) ) ;
#20820 = CARTESIAN_POINT ( 'NONE',  ( 68.45000000109247651, 7.933012699999995476, 14.99999999999999645 ) ) ;
#20821 = CARTESIAN_POINT ( 'NONE',  ( -3.458734124999998993, 0.000000000000000000, 13.43750000136560452 ) ) ;
#20822 = CIRCLE ( 'NONE', #3241, 6.735000000000022524 ) ;
#20823 = CARTESIAN_POINT ( 'NONE',  ( 2.499999999999999556, -7.958834565716820464, 7.593217523260554103 ) ) ;
#20824 = AXIS2_PLACEMENT_3D ( 'NONE', #16759, #13070, #22123 ) ;
#20825 = DIRECTION ( 'NONE',  ( -1.000000000000000000, -0.000000000000000000, -0.000000000000000000 ) ) ;
#20826 = EDGE_LOOP ( 'NONE', ( #19749, #10300, #9320, #8674, #10749, #2479, #18320, #5110, #20138, #18671, #22817, #20024, #5748, #9126 ) ) ;
#20827 = CARTESIAN_POINT ( 'NONE',  ( -4.000000000000000000, -1.656854249492383246, 2.362500000000002043 ) ) ;
#20828 = CARTESIAN_POINT ( 'NONE',  ( 69.40000000218495302, 9.999999999999998224, 17.49999999999999645 ) ) ;
#20829 = CARTESIAN_POINT ( 'NONE',  ( 4.999999999999999112, -4.762163868918343645, 9.915734732513202587 ) ) ;
#20830 = CARTESIAN_POINT ( 'NONE',  ( 2.500000000000000000, 0.000000000000000000, 0.000000000000000000 ) ) ;
#20831 = EDGE_CURVE ( 'NONE', #9234, #4247, #9856, .T. ) ;
#20832 = ORIENTED_EDGE ( 'NONE', *, *, #11992, .F. ) ;
#20833 = CARTESIAN_POINT ( 'NONE',  ( -66.00000000109247367, 9.143825827087052716, 12.93301269999999192 ) ) ;
#20834 = ORIENTED_EDGE ( 'NONE', *, *, #9095, .T. ) ;
#20835 = CARTESIAN_POINT ( 'NONE',  ( -68.90000000109246514, 12.06698730000000275, 15.85617417291294196 ) ) ;
#20836 = ORIENTED_EDGE ( 'NONE', *, *, #4539, .T. ) ;
#20837 = CARTESIAN_POINT ( 'NONE',  ( -1.656854249492380582, 4.000000000000000000, -1.762499997268811569 ) ) ;
#20838 = ORIENTED_EDGE ( 'NONE', *, *, #16986, .T. ) ;
#20839 = ORIENTED_EDGE ( 'NONE', *, *, #15860, .F. ) ;
#20840 = CARTESIAN_POINT ( 'NONE',  ( 2.445694354108822299, -2.445694354108820079, 17.06250000136560629 ) ) ;
#20841 = CARTESIAN_POINT ( 'NONE',  ( -65.75000000109245946, 9.999999999999998224, 17.06698730000000097 ) ) ;
#20842 = AXIS2_PLACEMENT_3D ( 'NONE', #12607, #217, #14630 ) ;
#20843 = CARTESIAN_POINT ( 'NONE',  ( -68.25000000109247367, 7.933012699999995476, 14.99999999999999645 ) ) ;
#20844 = CIRCLE ( 'NONE', #23540, 8.749000000000002331 ) ;
#20845 = CARTESIAN_POINT ( 'NONE',  ( 69.35000000109248219, 11.46158073645647235, 13.53841926354352232 ) ) ;
#20846 = CARTESIAN_POINT ( 'NONE',  ( -66.45000000109246230, 12.06698730000000097, 14.99999999999999645 ) ) ;
#20847 = DIRECTION ( 'NONE',  ( 0.3420201433256622736, -0.9396926207859106484, -1.232595164407828100E-31 ) ) ;
#20848 = CARTESIAN_POINT ( 'NONE',  ( 58.18518183416157541, 10.06805114094562548, 11.99999999999999645 ) ) ;
#20849 = CARTESIAN_POINT ( 'NONE',  ( 0.000000000000000000, 2.357898499370431722, -2.818925648462311528E-15 ) ) ;
#20850 = CARTESIAN_POINT ( 'NONE',  ( 6.353591512924457348E-16, -3.458734125000000770, 2.237500001365596791 ) ) ;
#20851 = LINE ( 'NONE', #13830, #15494 ) ;
#20852 = CARTESIAN_POINT ( 'NONE',  ( 1.656854249492384135, -3.999999999999999112, 10.43750000273119660 ) ) ;
#20853 = CARTESIAN_POINT ( 'NONE',  ( 4.999999999999999112, -9.241976615262146311, -1.699438267350473097 ) ) ;
#20854 = VERTEX_POINT ( 'NONE', #11552 ) ;
#20855 = DIRECTION ( 'NONE',  ( 1.224646799147353207E-16, -0.000000000000000000, 1.000000000000000000 ) ) ;
#20856 = ORIENTED_EDGE ( 'NONE', *, *, #12301, .T. ) ;
#20857 = CARTESIAN_POINT ( 'NONE',  ( 60.81018183416157541, 12.99999999999999822, 15.06805114094562192 ) ) ;
#20858 = VECTOR ( 'NONE', #7233, 1000.000000000000000 ) ;
#20859 = DIRECTION ( 'NONE',  ( 1.000000000000000000, 0.000000000000000000, 0.000000000000000000 ) ) ;
#20860 = CARTESIAN_POINT ( 'NONE',  ( 3.458734125000000326, 1.432654583217640498, 0.3000000013655960696 ) ) ;
#20861 = CARTESIAN_POINT ( 'NONE',  ( -2.445694354108820523, 2.445694354108820523, 0.6125000013655953479 ) ) ;
#20862 = ORIENTED_EDGE ( 'NONE', *, *, #15438, .T. ) ;
#20863 = CARTESIAN_POINT ( 'NONE',  ( 9.920644283265380691E-16, 4.000000000000000000, 14.75000000000000888 ) ) ;
#20864 = CARTESIAN_POINT ( 'NONE',  ( 4.000000000000000888, 4.898587196589412829E-16, 21.31370849898476649 ) ) ;
#20865 = ORIENTED_EDGE ( 'NONE', *, *, #23031, .F. ) ;
#20866 = EDGE_CURVE ( 'NONE', #2595, #2520, #15378, .T. ) ;
#20867 = CARTESIAN_POINT ( 'NONE',  ( -69.00000000218494733, 9.999999999999998224, 12.49999999999999289 ) ) ;
#20868 = CARTESIAN_POINT ( 'NONE',  ( -3.458734125000000770, 1.432654583217640498, -3.074999998634403209 ) ) ;
#20869 = CARTESIAN_POINT ( 'NONE',  ( 10.15255810323380992, -9.000000000000003553, 5.000000000000079936 ) ) ;
#20870 = CARTESIAN_POINT ( 'NONE',  ( 66.24999999999998579, 7.499999999999995559, 16.03553390593273420 ) ) ;
#20871 = EDGE_CURVE ( 'NONE', #7229, #15755, #20723, .T. ) ;
#20872 = CARTESIAN_POINT ( 'NONE',  ( 4.999999999999999112, -8.734705317681623171, -0.4999240074895356933 ) ) ;
#20873 = CARTESIAN_POINT ( 'NONE',  ( 70.85000000109246798, 9.999999999999998224, 12.93301269999999192 ) ) ;
#20874 = DIRECTION ( 'NONE',  ( -0.9413949561959078505, -0.3373062947069097040, 0.000000000000000000 ) ) ;
#20875 = CARTESIAN_POINT ( 'NONE',  ( 53.75231816583844591, 7.926799079670502124, 17.16943976678978245 ) ) ;
#20876 = CARTESIAN_POINT ( 'NONE',  ( 3.458734125000000326, 4.235727675282971730E-16, -2.762499998634404097 ) ) ;
#20877 = CARTESIAN_POINT ( 'NONE',  ( -3.458734124999998993, -1.432654583217642497, 10.75000000136560452 ) ) ;
#20878 = DIRECTION ( 'NONE',  ( 1.000000000000000000, 0.000000000000000000, 0.000000000000000000 ) ) ;
#20879 = CARTESIAN_POINT ( 'NONE',  ( -68.70000000109247651, 10.85617417291294551, 12.93301269999999192 ) ) ;
#20880 = CARTESIAN_POINT ( 'NONE',  ( -69.85000000218497007, 11.03553390593272177, 12.49999999999998046 ) ) ;
#20881 = DIRECTION ( 'NONE',  ( -1.000000000000000000, 0.000000000000000000, 0.000000000000000000 ) ) ;
#20882 = ORIENTED_EDGE ( 'NONE', *, *, #4429, .F. ) ;
#20883 = CARTESIAN_POINT ( 'NONE',  ( 1.656854249492384135, -3.999999999999999112, 14.31250000000001066 ) ) ;
#20884 =( BOUNDED_CURVE ( )  B_SPLINE_CURVE ( 2, ( #6343, #4534, #17712, #10546, #5235, #4885, #16037, #19254, #19364 ),
 .UNSPECIFIED., .F., .F. ) 
 B_SPLINE_CURVE_WITH_KNOTS ( ( 3, 2, 2, 2, 3 ),
 ( 0.4999999999999991118, 0.5156249999999995559, 0.5312500000000000000, 0.5468750000000004441, 0.5625000000000008882 ),
 .UNSPECIFIED. ) 
 CURVE ( )  GEOMETRIC_REPRESENTATION_ITEM ( )  RATIONAL_B_SPLINE_CURVE ( ( 1.000000000000004219, 0.9238795325112824086, 1.000000000000000000, 0.9238795325112867385, 1.000000000000000000, 0.9238795325112867385, 1.000000000000000000, 0.9238795325112824086, 1.000000000000004219 ) ) 
 REPRESENTATION_ITEM ( '' )  );
#20885 = CARTESIAN_POINT ( 'NONE',  ( 41.55923975928345016, -8.974600000000002353, 5.000000000000079936 ) ) ;
#20886 = ORIENTED_EDGE ( 'NONE', *, *, #22567, .F. ) ;
#20887 = ORIENTED_EDGE ( 'NONE', *, *, #23627, .F. ) ;
#20888 = CARTESIAN_POINT ( 'NONE',  ( -27.50000000000000711, 1.500000000000003109, -36.31025403784446581 ) ) ;
#20889 = CARTESIAN_POINT ( 'NONE',  ( -55.00000000000000000, 15.00000000000000000, 10.00000000000001599 ) ) ;
#20890 = ORIENTED_EDGE ( 'NONE', *, *, #10726, .F. ) ;
#20891 = DIRECTION ( 'NONE',  ( -0.000000000000000000, -0.000000000000000000, 1.000000000000000000 ) ) ;
#20892 = EDGE_CURVE ( 'NONE', #8470, #12358, #19716, .T. ) ;
#20893 = EDGE_CURVE ( 'NONE', #19953, #4600, #17695, .T. ) ;
#20894 = CARTESIAN_POINT ( 'NONE',  ( 67.05000000109247082, 12.06698730000000097, 14.99999999999999645 ) ) ;
#20895 = CARTESIAN_POINT ( 'NONE',  ( 67.50000000109245946, 9.143825827087049163, 17.06698729999999742 ) ) ;
#20896 = ADVANCED_FACE ( 'NONE', ( #2989 ), #13258, .T. ) ;
#20897 = VERTEX_POINT ( 'NONE', #1667 ) ;
#20898 = ADVANCED_FACE ( 'NONE', ( #10343 ), #1549, .T. ) ;
#20899 = AXIS2_PLACEMENT_3D ( 'NONE', #1789, #5278, #10740 ) ;
#20900 = LINE ( 'NONE', #10173, #6112 ) ;
#20901 = CARTESIAN_POINT ( 'NONE',  ( 56.62500000000000000, 12.82842712474620228, 17.82842712474617386 ) ) ;
#20902 = DIRECTION ( 'NONE',  ( -0.9396926207859107594, -0.3420201433256623291, 1.540743955509804830E-32 ) ) ;
#20903 = CARTESIAN_POINT ( 'NONE',  ( -2.445694354108819191, 2.445694354108820523, 18.31250000136560274 ) ) ;
#20904 = PLANE ( 'NONE',  #20071 ) ;
#20905 = VECTOR ( 'NONE', #11400, 1000.000000000000000 ) ;
#20906 = CARTESIAN_POINT ( 'NONE',  ( -20.00000000000001066, 7.500000000000001776, -49.99999999999998579 ) ) ;
#20907 = ORIENTED_EDGE ( 'NONE', *, *, #13083, .T. ) ;
#20908 = CARTESIAN_POINT ( 'NONE',  ( 9.000000000000000000, 0.000000000000000000, -4.000000000000000888 ) ) ;
#20909 = CARTESIAN_POINT ( 'NONE',  ( -70.59999999999999432, 11.76776695296636888, 13.23223304703362579 ) ) ;
#20910 = CIRCLE ( 'NONE', #20545, 4.000000000000000888 ) ;
#20911 = VERTEX_POINT ( 'NONE', #15731 ) ;
#20912 = PLANE ( 'NONE',  #20449 ) ;
#20913 = CARTESIAN_POINT ( 'NONE',  ( 5.384454397937118664, 0.000000000000000000, -5.000000000000000000 ) ) ;
#20914 = CARTESIAN_POINT ( 'NONE',  ( 65.00000000000000000, -15.00000000000000000, 10.00000000000007105 ) ) ;
#20915 = EDGE_CURVE ( 'NONE', #21411, #3496, #17850, .T. ) ;
#20916 = CARTESIAN_POINT ( 'NONE',  ( -6.500000000000000000, -3.752776749732573247, -0.5805565836007695601 ) ) ;
#20917 = VERTEX_POINT ( 'NONE', #12611 ) ;
#20918 = ORIENTED_EDGE ( 'NONE', *, *, #16909, .F. ) ;
#20919 = DIRECTION ( 'NONE',  ( 0.000000000000000000, 0.000000000000000000, -1.000000000000000000 ) ) ;
#20920 = EDGE_CURVE ( 'NONE', #11384, #10460, #3277, .T. ) ;
#20921 = CARTESIAN_POINT ( 'NONE',  ( -69.80000000218494449, 9.999999999999998224, 12.49999999999999289 ) ) ;
#20922 = CARTESIAN_POINT ( 'NONE',  ( 70.65000000218496723, 11.03553390593273598, 12.49999999999999289 ) ) ;
#20923 = CIRCLE ( 'NONE', #6811, 8.749000000000002331 ) ;
#20924 = CARTESIAN_POINT ( 'NONE',  ( -2.171643655288372443, 3.365003104552320767, 2.541098841762897165E-18 ) ) ;
#20925 = CARTESIAN_POINT ( 'NONE',  ( 66.45000000109246230, 12.06698730000000097, 14.99999999999999645 ) ) ;
#20926 = ADVANCED_FACE ( 'NONE', ( #8641 ), #21421, .T. ) ;
#20927 = ORIENTED_EDGE ( 'NONE', *, *, #20061, .F. ) ;
#20928 = AXIS2_PLACEMENT_3D ( 'NONE', #6777, #3293, #12423 ) ;
#20929 = AXIS2_PLACEMENT_3D ( 'NONE', #1519, #8503, #17710 ) ;
#20930 = EDGE_CURVE ( 'NONE', #20461, #16525, #12129, .T. ) ;
#20931 = CARTESIAN_POINT ( 'NONE',  ( -15.58579410928343911, -8.974600000000002353, 10.00000000000008882 ) ) ;
#20932 = CARTESIAN_POINT ( 'NONE',  ( -2.000000000000000888, 0.000000000000000000, -6.200000000000020606 ) ) ;
#20933 = CARTESIAN_POINT ( 'NONE',  ( 71.15000000109246514, 11.46158073645647235, 13.53841926354352232 ) ) ;
#20934 = CARTESIAN_POINT ( 'NONE',  ( -2.445694354108818303, -2.445694354108820523, 11.56250000136560629 ) ) ;
#20935 = LINE ( 'NONE', #16906, #17024 ) ;
#20936 = FACE_OUTER_BOUND ( 'NONE', #4353, .T. ) ;
#20937 = ORIENTED_EDGE ( 'NONE', *, *, #4130, .T. ) ;
#20938 = CARTESIAN_POINT ( 'NONE',  ( 4.000000000000000888, -1.656854249492379694, -0.2624999999999966804 ) ) ;
#20939 = DIRECTION ( 'NONE',  ( -1.000000000000000000, -0.000000000000000000, -0.000000000000000000 ) ) ;
#20940 = CARTESIAN_POINT ( 'NONE',  ( 25.00005080000000035, 0.000000000000000000, 4.000000000000000000 ) ) ;
#20941 = DIRECTION ( 'NONE',  ( -1.000000000000000000, -7.703719777548943412E-32, 0.000000000000000000 ) ) ;
#20942 = EDGE_LOOP ( 'NONE', ( #2608, #2347, #10087 ) ) ;
#20943 = CIRCLE ( 'NONE', #1070, 8.239200000000002078 ) ;
#20944 = DIRECTION ( 'NONE',  ( 0.3420201433256622181, 0.9396926207859107594, -6.162975822039141593E-32 ) ) ;
#20945 = ORIENTED_EDGE ( 'NONE', *, *, #13484, .T. ) ;
#20946 = CARTESIAN_POINT ( 'NONE',  ( -68.50000000109245946, 7.933012699999995476, 14.14382582708705094 ) ) ;
#20947 = VERTEX_POINT ( 'NONE', #14030 ) ;
#20948 = CARTESIAN_POINT ( 'NONE',  ( -19.99999999999999645, -9.000000000000003553, 5.000000000000079936 ) ) ;
#20949 = ORIENTED_EDGE ( 'NONE', *, *, #11790, .F. ) ;
#20950 = VECTOR ( 'NONE', #868, 1000.000000000000000 ) ;
#20951 = ORIENTED_EDGE ( 'NONE', *, *, #10668, .F. ) ;
#20952 = CARTESIAN_POINT ( 'NONE',  ( -2.445694354108818303, -2.445694354108820967, 14.81250000136560452 ) ) ;
#20953 = DIRECTION ( 'NONE',  ( 1.000000000000000000, -0.000000000000000000, -0.000000000000000000 ) ) ;
#20954 = DIRECTION ( 'NONE',  ( -1.000000000000000000, -0.000000000000000000, -0.000000000000000000 ) ) ;
#20955 = CARTESIAN_POINT ( 'NONE',  ( 66.80000000109247082, 9.143825827087052716, 12.93301269999999192 ) ) ;
#20956 = EDGE_CURVE ( 'NONE', #19596, #4473, #21626, .T. ) ;
#20957 = EDGE_CURVE ( 'NONE', #8889, #8094, #2699, .T. ) ;
#20958 = AXIS2_PLACEMENT_3D ( 'NONE', #10791, #23450, #21758 ) ;
#20959 = CARTESIAN_POINT ( 'NONE',  ( -67.80000000109247082, 9.143825827087050939, 12.93301269999999370 ) ) ;
#20960 = CARTESIAN_POINT ( 'NONE',  ( -71.34999999999999432, 11.03553390593268269, 12.49999999999994138 ) ) ;
#20961 = CARTESIAN_POINT ( 'NONE',  ( 59.21643183416158962, 12.97181229448535689, 16.31069182806490758 ) ) ;
#20962 = CARTESIAN_POINT ( 'NONE',  ( 0.000000000000000000, -4.729683950898817102, -7.360373001730970977 ) ) ;
#20963 = AXIS2_PLACEMENT_3D ( 'NONE', #5951, #20891, #18991 ) ;
#20964 = CARTESIAN_POINT ( 'NONE',  ( 2.445694354108820079, 2.445694354108820523, 3.612500001365598123 ) ) ;
#20965 = CARTESIAN_POINT ( 'NONE',  ( 0.000000000000000000, -8.475820894092946034, -4.057423117305485327 ) ) ;
#20966 = CARTESIAN_POINT ( 'NONE',  ( -1.656854249492379250, 4.000000000000000000, 11.93750000273119660 ) ) ;
#20967 = CARTESIAN_POINT ( 'NONE',  ( -60.00000000000000711, 9.999999999999998224, 12.49999999999999289 ) ) ;
#20968 = ORIENTED_EDGE ( 'NONE', *, *, #17979, .F. ) ;
#20969 = CARTESIAN_POINT ( 'NONE',  ( 9.920644283265380691E-16, 4.000000000000000000, 16.87500000273119838 ) ) ;
#20970 = ORIENTED_EDGE ( 'NONE', *, *, #5419, .F. ) ;
#20971 = CARTESIAN_POINT ( 'NONE',  ( 53.12268183416157541, 12.07320092032950676, 17.16943976678977180 ) ) ;
#20972 = SURFACE_STYLE_FILL_AREA ( #1098 ) ;
#20973 = CARTESIAN_POINT ( 'NONE',  ( -3.458734125000000326, 0.000000000000000000, 0.7375000013655954589 ) ) ;
#20974 = VECTOR ( 'NONE', #14532, 1000.000000000000114 ) ;
#20975 = CARTESIAN_POINT ( 'NONE',  ( 1.432654583217642053, -3.458734124999999437, -0.9499999986344030978 ) ) ;
#20976 = ORIENTED_EDGE ( 'NONE', *, *, #11701, .T. ) ;
#20977 = CARTESIAN_POINT ( 'NONE',  ( -10.13078668033273999, -11.25000000000000355, 10.00000000000008882 ) ) ;
#20978 = CONICAL_SURFACE ( 'NONE', #8773, 2.055000000000000160, 0.7853981633974639331 ) ;
#20979 = EDGE_LOOP ( 'NONE', ( #16466, #14065, #4906, #3088 ) ) ;
#20980 = CARTESIAN_POINT ( 'NONE',  ( 1.799999999999996048, 0.000000000000000000, 0.000000000000000000 ) ) ;
#20981 = ORIENTED_EDGE ( 'NONE', *, *, #11603, .F. ) ;
#20982 = PRODUCT_DEFINITION_SHAPE ( 'NONE', 'NONE',  #7275 ) ;
#20983 = CARTESIAN_POINT ( 'NONE',  ( 50.00231816583843170, 12.78030770151603868, 12.12345345202365188 ) ) ;
#20984 = PRODUCT_DEFINITION_FORMATION_WITH_SPECIFIED_SOURCE ( 'ANY', '', #908, .NOT_KNOWN. ) ;
#20985 = CARTESIAN_POINT ( 'NONE',  ( -70.55000000218495870, 8.964466094067258695, 12.49999999999999289 ) ) ;
#20986 = AXIS2_PLACEMENT_3D ( 'NONE', #1494, #10163, #19576 ) ;
#20987 = CARTESIAN_POINT ( 'NONE',  ( 0.000000000000000000, -6.772677083992345359, -5.538577986808975062 ) ) ;
#20988 = CARTESIAN_POINT ( 'NONE',  ( -20.00000000000001066, 1.500000000000003109, -50.00000000000000000 ) ) ;
#20989 = CARTESIAN_POINT ( 'NONE',  ( 3.458734125000001658, 1.432654583217640498, 19.25000000136560629 ) ) ;
#20990 = VECTOR ( 'NONE', #23569, 1000.000000000000000 ) ;
#20991 = LINE ( 'NONE', #4610, #23457 ) ;
#20992 = CARTESIAN_POINT ( 'NONE',  ( 69.65000000109247935, 9.999999999999998224, 17.06698730000000097 ) ) ;
#20993 = CIRCLE ( 'NONE', #10725, 6.500000000000000888 ) ;
#20994 = LINE ( 'NONE', #13499, #6136 ) ;
#20995 = CARTESIAN_POINT ( 'NONE',  ( 52.53356816583844591, 11.31069182806492712, 17.97181229448534623 ) ) ;
#20996 = CARTESIAN_POINT ( 'NONE',  ( 2.445694354108820967, -2.445694354108820079, 3.362500001365597679 ) ) ;
#20997 = CARTESIAN_POINT ( 'NONE',  ( -3.458734124999999437, 0.000000000000000000, 12.68750000136560629 ) ) ;
#20998 = DIRECTION ( 'NONE',  ( 0.000000000000000000, 0.000000000000000000, 1.000000000000000000 ) ) ;
#20999 = CARTESIAN_POINT ( 'NONE',  ( -67.75000000109245946, 8.538419263543524096, 13.53841926354352054 ) ) ;
#21000 = ADVANCED_FACE ( 'NONE', ( #5268 ), #12251, .T. ) ;
#21001 = DIRECTION ( 'NONE',  ( -0.000000000000000000, -1.000000000000000000, -0.000000000000000000 ) ) ;
#21002 = CARTESIAN_POINT ( 'NONE',  ( -69.74999999999998579, 11.03553390593276262, 12.50000000000001776 ) ) ;
#21003 = ORIENTED_EDGE ( 'NONE', *, *, #8948, .T. ) ;
#21004 = CARTESIAN_POINT ( 'NONE',  ( -1.519999999999999574, 0.000000000000000000, -6.760799999999997034 ) ) ;
#21006 = AXIS2_PLACEMENT_3D ( 'NONE', #1476, #12660, #17782 ) ;
#21005 = SURFACE_STYLE_USAGE ( .BOTH. , #3163 ) ;
#21007 = CARTESIAN_POINT ( 'NONE',  ( -1.656854249492381248, -3.999999999999999112, 3.612500002731187099 ) ) ;
#21008 = ORIENTED_EDGE ( 'NONE', *, *, #11253, .F. ) ;
#21009 = ORIENTED_EDGE ( 'NONE', *, *, #479, .F. ) ;
#21010 = DIRECTION ( 'NONE',  ( 1.224646799147353207E-16, -0.000000000000000000, 1.000000000000000000 ) ) ;
#21011 = CARTESIAN_POINT ( 'NONE',  ( 52.40625000000000000, 13.99999999999999289, 13.34314575050759544 ) ) ;
#21012 = VERTEX_POINT ( 'NONE', #16182 ) ;
#21013 = LINE ( 'NONE', #8482, #17191 ) ;
#21014 = CIRCLE ( 'NONE', #13403, 2.100000000000000089 ) ;
#21015 = CARTESIAN_POINT ( 'NONE',  ( 66.90000000109246514, 10.85617417291294551, 12.93301269999999370 ) ) ;
#21016 = VECTOR ( 'NONE', #11513, 1000.000000000000000 ) ;
#21017 = VECTOR ( 'NONE', #9148, 1000.000000000000000 ) ;
#21018 = CARTESIAN_POINT ( 'NONE',  ( 68.85000000109246798, 12.06698730000000097, 14.99999999999999645 ) ) ;
#21019 = ORIENTED_EDGE ( 'NONE', *, *, #8502, .F. ) ;
#21020 = CARTESIAN_POINT ( 'NONE',  ( 4.999999999999999112, -6.478011392632841314, -6.807171995660652897 ) ) ;
#21021 =( BOUNDED_CURVE ( )  B_SPLINE_CURVE ( 2, ( #10190, #3200, #8611, #21265, #12102, #23193, #14251, #6807, #23325 ),
 .UNSPECIFIED., .F., .F. ) 
 B_SPLINE_CURVE_WITH_KNOTS ( ( 3, 2, 2, 2, 3 ),
 ( 0.4374999999999995004, 0.4531249999999993894, 0.4687499999999993339, 0.4843749999999992228, 0.4999999999999991118 ),
 .UNSPECIFIED. ) 
 CURVE ( )  GEOMETRIC_REPRESENTATION_ITEM ( )  RATIONAL_B_SPLINE_CURVE ( ( 1.000000000000002442, 0.9238795325112842960, 1.000000000000000000, 0.9238795325112867385, 1.000000000000000000, 0.9238795325112867385, 1.000000000000000000, 0.9238795325112910684, 0.9999999999999956701 ) ) 
 REPRESENTATION_ITEM ( '' )  );
#21022 = CARTESIAN_POINT ( 'NONE',  ( 58.40625000000000711, 13.99999999999999289, 13.34314575050759544 ) ) ;
#21023 = CARTESIAN_POINT ( 'NONE',  ( -3.250000000000004885, -5.629165124598848990, -3.700000000000000178 ) ) ;
#21024 = CARTESIAN_POINT ( 'NONE',  ( -3.458734124999998993, 0.000000000000000000, 18.43750000136560629 ) ) ;
#21025 = CARTESIAN_POINT ( 'NONE',  ( 65.00000000000000000, 15.00000000000000000, 24.99999999999999645 ) ) ;
#21026 = ADVANCED_FACE ( 'NONE', ( #7080, #14395 ), #23108, .T. ) ;
#21027 = CARTESIAN_POINT ( 'NONE',  ( 0.000000000000000000, 0.000000000000000000, 0.000000000000000000 ) ) ;
#21028 = ORIENTED_EDGE ( 'NONE', *, *, #6110, .T. ) ;
#21029 = EDGE_CURVE ( 'NONE', #8317, #16789, #6396, .T. ) ;
#21030 = PLANE ( 'NONE',  #15553 ) ;
#21031 = FACE_OUTER_BOUND ( 'NONE', #920, .T. ) ;
#21032 = VECTOR ( 'NONE', #22254, 1000.000000000000000 ) ;
#21033 = EDGE_LOOP ( 'NONE', ( #10894, #22280, #5300, #7771, #23326, #3530 ) ) ;
#21034 = PLANE ( 'NONE',  #3632 ) ;
#21035 = CARTESIAN_POINT ( 'NONE',  ( 4.211140560182196957, -2.431303136016555122, -3.745885042887436622 ) ) ;
#21036 = DIRECTION ( 'NONE',  ( -1.000000000000000000, 0.000000000000000000, 1.224646799147353454E-16 ) ) ;
#21037 = PRODUCT_DEFINITION_CONTEXT ( 'detailed design', #3804, 'design' ) ;
#21038 = ADVANCED_FACE ( 'NONE', ( #11390 ), #6485, .F. ) ;
#21039 = PLANE ( 'NONE',  #4109 ) ;
#21040 = ORIENTED_EDGE ( 'NONE', *, *, #12347, .F. ) ;
#21041 = CARTESIAN_POINT ( 'NONE',  ( -4.000000000000000888, 1.656854249492380582, 1.237500000000000488 ) ) ;
#21042 = ORIENTED_EDGE ( 'NONE', *, *, #6137, .T. ) ;
#21043 = CARTESIAN_POINT ( 'NONE',  ( 0.000000000000000000, 4.729683950898977862, -7.360373001730867060 ) ) ;
#21044 = CARTESIAN_POINT ( 'NONE',  ( -3.999999999999999112, 0.000000000000000000, 21.31370849898476649 ) ) ;
#21045 = CARTESIAN_POINT ( 'NONE',  ( 1.600000000000004086, 0.000000000000000000, -8.265000000000021885 ) ) ;
#21046 = DIRECTION ( 'NONE',  ( 0.000000000000000000, 0.000000000000000000, 1.000000000000000000 ) ) ;
#21047 = CARTESIAN_POINT ( 'NONE',  ( 66.20000000109246230, 9.143825827087052716, 12.93301269999999192 ) ) ;
#21048 = ORIENTED_EDGE ( 'NONE', *, *, #14642, .F. ) ;
#21049 = AXIS2_PLACEMENT_3D ( 'NONE', #205, #9108, #1996 ) ;
#21050 = CARTESIAN_POINT ( 'NONE',  ( -3.999999999999999112, 0.000000000000000000, 10.12500000273119660 ) ) ;
#21051 = EDGE_CURVE ( 'NONE', #21587, #19809, #22128, .T. ) ;
#21052 = FACE_OUTER_BOUND ( 'NONE', #7192, .T. ) ;
#21053 = CARTESIAN_POINT ( 'NONE',  ( 68.50000000109245946, 7.933012699999995476, 14.14382582708705094 ) ) ;
#21054 = CARTESIAN_POINT ( 'NONE',  ( 2.445694354108821411, 2.445694354108820523, 13.06250000136560452 ) ) ;
#21055 = DIRECTION ( 'NONE',  ( 1.000000000000000000, 0.000000000000000000, -1.224646799147353207E-16 ) ) ;
#21056 = FACE_OUTER_BOUND ( 'NONE', #15509, .T. ) ;
#21057 = ORIENTED_EDGE ( 'NONE', *, *, #6365, .F. ) ;
#21058 = CARTESIAN_POINT ( 'NONE',  ( 1.656854249492380360, 4.000000000000000000, -2.012499999999997957 ) ) ;
#21059 = EDGE_CURVE ( 'NONE', #23518, #3912, #18319, .T. ) ;
#21060 = PLANE ( 'NONE',  #4808 ) ;
#21061 = CYLINDRICAL_SURFACE ( 'NONE', #13914, 11.00000000000000000 ) ;
#21062 = CARTESIAN_POINT ( 'NONE',  ( 0.2500000000000002220, 0.000000000000000000, 4.250000000000000000 ) ) ;
#21063 =( BOUNDED_SURFACE ( )  B_SPLINE_SURFACE ( 3, 2, ( 
 ( #17551, #12406, #4836, #12295, #8812, #21107, #23394, #1229, #10384, #1348, #8567, #16110, #6533, #14201, #8460, #4722, #15875, #12531, #6999, #6761, #15767, #3152, #12055, #19321, #8684, #19558, #13962, #23038, #21221, #10496, #15986, #5190, #23273, #21461, #1469, #6881, #12167, #17891, #10619, #2910, #5074, #19671, #10739, #3276, #14318, #3393, #2053, #20018, #3515, #7367, #14562, #16457, #1820, #16222, #3865, #21826, #18124, #1590, #19913, #3981, #23508, #1943, #22173, #11319, #13116, #10848, #7479, #1703, #5787, #5312, #9170, #18237, #21935, #3620, #7122, #14675, #36, #8928, #9047, #148, #18474, #14435, #7246, #11076, #10960, #21701, #5543, #20375, #12875, #22043, #20130, #14795, #5430, #23633, #3736, #11200, #12996 ),
 ( #18362, #9395, #12652, #9282, #14915, #16337, #12766, #16568, #5661, #20260, #16688, #259, #7593, #2418, #4338, #11677, #18594, #13231, #6261, #20961, #9870, #2176, #18946, #13698, #9640, #22654, #2531, #2304, #17165, #19065, #20848, #17289, #7722, #2657, #15035, #16931, #745, #4455, #20619, #15269, #5906, #8080, #13581, #4581, #6149, #11441, #15391, #9513, #18716, #15151, #508, #11794, #18832, #16811, #9999, #7830, #22412, #391, #20497, #22292, #4101, #855, #15501, #6022, #6381, #13350, #8188, #4226, #22771, #11562, #9749, #17047, #22540, #622, #7949, #13472, #20732, #19185, #21082, #10796, #5373, #17403, #17519, #21642, #6618, #2770, #1531, #7312, #23453, #8994, #5131, #1650, #15744, #10228, #14261, #14500, #23577 ),
 ( #12715, #10111, #18070, #12028, #969, #19731, #16397, #10905, #3332, #4694, #7061, #15622, #8301, #16284, #23694, #19292, #14618, #3569, #19967, #21879, #21521, #7185, #12469, #5248, #22891, #11917, #18185, #1086, #2881, #16167, #12595, #6506, #13826, #19853, #1766, #8431, #23013, #10675, #17951, #8873, #14381, #3458, #21764, #9107, #20314, #3915, #20197, #12933, #204, #20079, #9228, #11017, #4161, #13059, #11254, #7885, #21992, #7535, #11507, #16988, #2360, #1884, #18779, #18527, #2114, #14852, #5964, #22107, #5606, #16873, #9449, #5486, #11142, #7657, #16626, #14980, #16745, #16514, #18303, #22348, #9691, #560, #12821, #326, #5727, #22233, #5841, #13168, #13288, #20434, #4043, #11373, #3679, #89, #450, #15204, #18651 ),
 ( #3806, #9580, #2240, #18416, #7775, #20555, #15093, #7423, #14733, #1995, #9336, #20790, #4637, #1028, #802, #19127, #9807, #21022, #17465, #8489, #10054, #15330, #22827, #6079, #22600, #18998, #4396, #15565, #6442, #17229, #11735, #674, #6204, #11851, #13762, #19351, #20901, #11971, #15682, #17344, #2587, #8364, #22955, #4282, #9932, #17098, #1148, #8009, #15445, #10174, #6563, #8134, #13522, #4514, #22712, #13638, #6323, #13411, #13879, #2713, #911, #22468, #8247, #20678, #11616, #19237, #2940, #18886, #10291, #2827, #21137, #4750, #17582, #2472, #12086, #8713, #12436, #17807, #6676, #21491, #16019, #23065, #1257, #14350, #8963, #21251, #21374, #1507, #10529, #13989, #5104, #10877, #3304, #12563, #23308, #5218, #19587 ),
 ( #3429, #10647, #19701, #4995, #17922, #16253, #4868, #8846, #7152, #16141, #5344, #21611, #12203, #23426, #7033, #8596, #19823, #12324, #10770, #23544, #19474, #14466, #1375, #3183, #18044, #6917, #21732, #3072, #1621, #15902, #10416, #14234, #19942, #12688, #3542, #23179, #18153, #17696, #6790, #1737, #15793, #14111, #4132, #421, #9547, #11474, #18388, #5813, #11110, #18499, #16367, #20524, #16843, #21962, #16486, #13028, #2084, #9076, #14593, #9425, #2208, #18750, #7280, #7394, #12795, #21853, #23663, #16714, #10987, #5693, #177, #7509, #62, #14706, #3770, #5459, #20047, #3651, #7748, #16598, #14822, #18266, #1851, #1968, #15063, #9200, #5934, #5575, #22319, #22074, #20288, #9308, #13261, #3889, #12902, #20404, #11225 ),
 ( #292, #20163, #7627, #14950, #22202, #13140, #4011, #11349, #18621, #18859, #2333, #20653, #4726, #16957, #2691, #22926, #12059, #13855, #4257, #8219, #2445, #6538, #6052, #2557, #18974, #22682, #4368, #534, #8111, #9905, #9667, #11591, #885, #19214, #7856, #15180, #7982, #4484, #13500, #11823, #15420, #13384, #22439, #2803, #9779, #6295, #10145, #17437, #13731, #1003, #21110, #17075, #778, #17200, #649, #13612, #20875, #19099, #20763, #15302, #15536, #22576, #6180, #11706, #10031, #17319, #22802, #6416, #8336, #20995, #4615, #11949, #15654, #23041, #10744, #21463, #8931, #17895, #2913, #5076, #1351, #4839, #23396, #15877, #8686, #19797, #1120, #18017, #4966, #6764, #12408, #14080, #3395, #17554, #1472, #19442, #8465 ),
 ( #3154, #12172, #14205, #6652, #15769, #16113, #23510, #3040, #14437, #1592, #16224, #21705, #12298, #7001, #21342, #19673, #10263, #7125, #5314, #8570, #10389, #23275, #3278, #19325, #13965, #10621, #12533, #21226, #17670, #1231, #23152, #19560, #10499, #8815, #17779, #15991, #6884, #14320, #21579, #5192, #7370, #3517, #16339, #18127, #11323, #20132, #11079, #15037, #5433, #14679, #18596, #393, #9518, #9049, #2179, #18365, #1946, #21937, #13118, #5545, #12768, #262, #9284, #20377, #12878, #14566, #16572, #1824, #3740, #151, #10850, #14919, #9173, #20020, #12656, #7248, #22294, #1705, #12997, #16814, #19917, #7724, #21830, #18476, #3623, #23637, #10962, #7481, #14797, #22046, #5665, #18239, #20263, #3868, #16460, #39, #11202 ) ),
 .UNSPECIFIED., .T., .F., .F. ) 
 B_SPLINE_SURFACE_WITH_KNOTS ( ( 4, 3, 4 ),
 ( 3, 2, 2, 2, 2, 2, 2, 2, 2, 2, 2, 2, 2, 2, 2, 2, 2, 2, 2, 2, 2, 2, 2, 2, 2, 2, 2, 2, 2, 2, 2, 2, 2, 2, 2, 2, 2, 2, 2, 2, 2, 2, 2, 2, 2, 2, 2, 2, 3 ),
 ( 0.000000000000000000, 0.5000000000000000000, 1.000000000000000000 ),
 ( 0.000000000000000000, 0.02083333333333333218, 0.04166666666666666435, 0.06250000000000000000, 0.08333333333333332871, 0.1041666666666666713, 0.1250000000000000000, 0.1458333333333333426, 0.1666666666666666574, 0.1875000000000000000, 0.2083333333333333426, 0.2291666666666666574, 0.2500000000000000000, 0.2708333333333333148, 0.2916666666666666852, 0.3125000000000000000, 0.3333333333333333148, 0.3541666666666666852, 0.3750000000000000000, 0.3958333333333333148, 0.4166666666666666852, 0.4375000000000000000, 0.4583333333333333148, 0.4791666666666666852, 0.5000000000000000000, 0.5208333333333333703, 0.5416666666666666297, 0.5625000000000000000, 0.5833333333333333703, 0.6041666666666666297, 0.6250000000000000000, 0.6458333333333333703, 0.6666666666666666297, 0.6875000000000000000, 0.7083333333333333703, 0.7291666666666666297, 0.7500000000000000000, 0.7708333333333333703, 0.7916666666666666297, 0.8125000000000000000, 0.8333333333333333703, 0.8541666666666666297, 0.8750000000000000000, 0.8958333333333333703, 0.9166666666666666297, 0.9375000000000000000, 0.9583333333333333703, 0.9791666666666666297, 1.000000000000000000 ),
 .UNSPECIFIED. ) 
 GEOMETRIC_REPRESENTATION_ITEM ( )  RATIONAL_B_SPLINE_SURFACE ( (
 ( 1.000000000000000000, 0.9238795325112867385, 1.000000000000000000, 0.9238795325112867385, 1.000000000000000000, 0.9238795325112867385, 1.000000000000000000, 0.9238795325112867385, 1.000000000000000000, 0.9238795325112867385, 1.000000000000000000, 0.9238795325112867385, 1.000000000000000000, 0.9238795325112867385, 1.000000000000000000, 0.9238795325112867385, 1.000000000000000000, 0.9238795325112867385, 1.000000000000000000, 0.9238795325112867385, 1.000000000000000000, 0.9238795325112867385, 1.000000000000000000, 0.9238795325112867385, 1.000000000000000000, 0.9238795325112867385, 1.000000000000000000, 0.9238795325112867385, 1.000000000000000000, 0.9238795325112867385, 1.000000000000000000, 0.9238795325112867385, 1.000000000000000000, 0.9238795325112867385, 1.000000000000000000, 0.9238795325112867385, 1.000000000000000000, 0.9238795325112867385, 1.000000000000000000, 0.9238795325112867385, 1.000000000000000000, 0.9238795325112867385, 1.000000000000000000, 0.9238795325112867385, 1.000000000000000000, 0.9238795325112867385, 1.000000000000000000, 0.9238795325112867385, 1.000000000000000000, 0.9238795325112867385, 1.000000000000000000, 0.9238795325112867385, 1.000000000000000000, 0.9238795325112867385, 1.000000000000000000, 0.9238795325112867385, 1.000000000000000000, 0.9238795325112867385, 1.000000000000000000, 0.9238795325112867385, 1.000000000000000000, 0.9238795325112867385, 1.000000000000000000, 0.9238795325112867385, 1.000000000000000000, 0.9238795325112867385, 1.000000000000000000, 0.9238795325112867385, 1.000000000000000000, 0.9238795325112867385, 1.000000000000000000, 0.9238795325112867385, 1.000000000000000000, 0.9238795325112867385, 1.000000000000000000, 0.9238795325112867385, 1.000000000000000000, 0.9238795325112867385, 1.000000000000000000, 0.9238795325112867385, 1.000000000000000000, 0.9238795325112867385, 1.000000000000000000, 0.9238795325112867385, 1.000000000000000000, 0.9238795325112867385, 1.000000000000000000, 0.9238795325112867385, 1.000000000000000000, 0.9238795325112867385, 1.000000000000000000, 0.9238795325112867385, 1.000000000000000000, 0.9238795325112867385, 1.000000000000000000, 0.9238795325112867385, 1.000000000000000000),
 ( 0.3333333333333333703, 0.3079598441704289313, 0.3333333333333333703, 0.3079598441704289313, 0.3333333333333333703, 0.3079598441704289313, 0.3333333333333333703, 0.3079598441704289313, 0.3333333333333333703, 0.3079598441704289313, 0.3333333333333333703, 0.3079598441704289313, 0.3333333333333333703, 0.3079598441704289313, 0.3333333333333333703, 0.3079598441704289313, 0.3333333333333333703, 0.3079598441704289313, 0.3333333333333333703, 0.3079598441704289313, 0.3333333333333333703, 0.3079598441704289313, 0.3333333333333333703, 0.3079598441704289313, 0.3333333333333333703, 0.3079598441704289313, 0.3333333333333333703, 0.3079598441704289313, 0.3333333333333333703, 0.3079598441704289313, 0.3333333333333333703, 0.3079598441704289313, 0.3333333333333333703, 0.3079598441704289313, 0.3333333333333333703, 0.3079598441704289313, 0.3333333333333333703, 0.3079598441704289313, 0.3333333333333333703, 0.3079598441704289313, 0.3333333333333333703, 0.3079598441704289313, 0.3333333333333333703, 0.3079598441704289313, 0.3333333333333333703, 0.3079598441704289313, 0.3333333333333333703, 0.3079598441704289313, 0.3333333333333333703, 0.3079598441704289313, 0.3333333333333333703, 0.3079598441704289313, 0.3333333333333333703, 0.3079598441704289313, 0.3333333333333333703, 0.3079598441704289313, 0.3333333333333333703, 0.3079598441704289313, 0.3333333333333333703, 0.3079598441704289313, 0.3333333333333333703, 0.3079598441704289313, 0.3333333333333333703, 0.3079598441704289313, 0.3333333333333333703, 0.3079598441704289313, 0.3333333333333333703, 0.3079598441704289313, 0.3333333333333333703, 0.3079598441704289313, 0.3333333333333333703, 0.3079598441704289313, 0.3333333333333333703, 0.3079598441704289313, 0.3333333333333333703, 0.3079598441704289313, 0.3333333333333333703, 0.3079598441704289313, 0.3333333333333333703, 0.3079598441704289313, 0.3333333333333333703, 0.3079598441704289313, 0.3333333333333333703, 0.3079598441704289313, 0.3333333333333333703, 0.3079598441704289313, 0.3333333333333333703, 0.3079598441704289313, 0.3333333333333333703, 0.3079598441704289313, 0.3333333333333333703, 0.3079598441704289313, 0.3333333333333333703, 0.3079598441704289313, 0.3333333333333333703, 0.3079598441704289313, 0.3333333333333333703),
 ( 0.3333333333333333703, 0.3079598441704289313, 0.3333333333333333703, 0.3079598441704289313, 0.3333333333333333703, 0.3079598441704289313, 0.3333333333333333703, 0.3079598441704289313, 0.3333333333333333703, 0.3079598441704289313, 0.3333333333333333703, 0.3079598441704289313, 0.3333333333333333703, 0.3079598441704289313, 0.3333333333333333703, 0.3079598441704289313, 0.3333333333333333703, 0.3079598441704289313, 0.3333333333333333703, 0.3079598441704289313, 0.3333333333333333703, 0.3079598441704289313, 0.3333333333333333703, 0.3079598441704289313, 0.3333333333333333703, 0.3079598441704289313, 0.3333333333333333703, 0.3079598441704289313, 0.3333333333333333703, 0.3079598441704289313, 0.3333333333333333703, 0.3079598441704289313, 0.3333333333333333703, 0.3079598441704289313, 0.3333333333333333703, 0.3079598441704289313, 0.3333333333333333703, 0.3079598441704289313, 0.3333333333333333703, 0.3079598441704289313, 0.3333333333333333703, 0.3079598441704289313, 0.3333333333333333703, 0.3079598441704289313, 0.3333333333333333703, 0.3079598441704289313, 0.3333333333333333703, 0.3079598441704289313, 0.3333333333333333703, 0.3079598441704289313, 0.3333333333333333703, 0.3079598441704289313, 0.3333333333333333703, 0.3079598441704289313, 0.3333333333333333703, 0.3079598441704289313, 0.3333333333333333703, 0.3079598441704289313, 0.3333333333333333703, 0.3079598441704289313, 0.3333333333333333703, 0.3079598441704289313, 0.3333333333333333703, 0.3079598441704289313, 0.3333333333333333703, 0.3079598441704289313, 0.3333333333333333703, 0.3079598441704289313, 0.3333333333333333703, 0.3079598441704289313, 0.3333333333333333703, 0.3079598441704289313, 0.3333333333333333703, 0.3079598441704289313, 0.3333333333333333703, 0.3079598441704289313, 0.3333333333333333703, 0.3079598441704289313, 0.3333333333333333703, 0.3079598441704289313, 0.3333333333333333703, 0.3079598441704289313, 0.3333333333333333703, 0.3079598441704289313, 0.3333333333333333703, 0.3079598441704289313, 0.3333333333333333703, 0.3079598441704289313, 0.3333333333333333703, 0.3079598441704289313, 0.3333333333333333703, 0.3079598441704289313, 0.3333333333333333703, 0.3079598441704289313, 0.3333333333333333703, 0.3079598441704289313, 0.3333333333333333703),
 ( 1.000000000000000000, 0.9238795325112867385, 1.000000000000000000, 0.9238795325112867385, 1.000000000000000000, 0.9238795325112867385, 1.000000000000000000, 0.9238795325112867385, 1.000000000000000000, 0.9238795325112867385, 1.000000000000000000, 0.9238795325112867385, 1.000000000000000000, 0.9238795325112867385, 1.000000000000000000, 0.9238795325112867385, 1.000000000000000000, 0.9238795325112867385, 1.000000000000000000, 0.9238795325112867385, 1.000000000000000000, 0.9238795325112867385, 1.000000000000000000, 0.9238795325112867385, 1.000000000000000000, 0.9238795325112867385, 1.000000000000000000, 0.9238795325112867385, 1.000000000000000000, 0.9238795325112867385, 1.000000000000000000, 0.9238795325112867385, 1.000000000000000000, 0.9238795325112867385, 1.000000000000000000, 0.9238795325112867385, 1.000000000000000000, 0.9238795325112867385, 1.000000000000000000, 0.9238795325112867385, 1.000000000000000000, 0.9238795325112867385, 1.000000000000000000, 0.9238795325112867385, 1.000000000000000000, 0.9238795325112867385, 1.000000000000000000, 0.9238795325112867385, 1.000000000000000000, 0.9238795325112867385, 1.000000000000000000, 0.9238795325112867385, 1.000000000000000000, 0.9238795325112867385, 1.000000000000000000, 0.9238795325112867385, 1.000000000000000000, 0.9238795325112867385, 1.000000000000000000, 0.9238795325112867385, 1.000000000000000000, 0.9238795325112867385, 1.000000000000000000, 0.9238795325112867385, 1.000000000000000000, 0.9238795325112867385, 1.000000000000000000, 0.9238795325112867385, 1.000000000000000000, 0.9238795325112867385, 1.000000000000000000, 0.9238795325112867385, 1.000000000000000000, 0.9238795325112867385, 1.000000000000000000, 0.9238795325112867385, 1.000000000000000000, 0.9238795325112867385, 1.000000000000000000, 0.9238795325112867385, 1.000000000000000000, 0.9238795325112867385, 1.000000000000000000, 0.9238795325112867385, 1.000000000000000000, 0.9238795325112867385, 1.000000000000000000, 0.9238795325112867385, 1.000000000000000000, 0.9238795325112867385, 1.000000000000000000, 0.9238795325112867385, 1.000000000000000000, 0.9238795325112867385, 1.000000000000000000, 0.9238795325112867385, 1.000000000000000000),
 ( 0.3333333333333333703, 0.3079598441704289313, 0.3333333333333333703, 0.3079598441704289313, 0.3333333333333333703, 0.3079598441704289313, 0.3333333333333333703, 0.3079598441704289313, 0.3333333333333333703, 0.3079598441704289313, 0.3333333333333333703, 0.3079598441704289313, 0.3333333333333333703, 0.3079598441704289313, 0.3333333333333333703, 0.3079598441704289313, 0.3333333333333333703, 0.3079598441704289313, 0.3333333333333333703, 0.3079598441704289313, 0.3333333333333333703, 0.3079598441704289313, 0.3333333333333333703, 0.3079598441704289313, 0.3333333333333333703, 0.3079598441704289313, 0.3333333333333333703, 0.3079598441704289313, 0.3333333333333333703, 0.3079598441704289313, 0.3333333333333333703, 0.3079598441704289313, 0.3333333333333333703, 0.3079598441704289313, 0.3333333333333333703, 0.3079598441704289313, 0.3333333333333333703, 0.3079598441704289313, 0.3333333333333333703, 0.3079598441704289313, 0.3333333333333333703, 0.3079598441704289313, 0.3333333333333333703, 0.3079598441704289313, 0.3333333333333333703, 0.3079598441704289313, 0.3333333333333333703, 0.3079598441704289313, 0.3333333333333333703, 0.3079598441704289313, 0.3333333333333333703, 0.3079598441704289313, 0.3333333333333333703, 0.3079598441704289313, 0.3333333333333333703, 0.3079598441704289313, 0.3333333333333333703, 0.3079598441704289313, 0.3333333333333333703, 0.3079598441704289313, 0.3333333333333333703, 0.3079598441704289313, 0.3333333333333333703, 0.3079598441704289313, 0.3333333333333333703, 0.3079598441704289313, 0.3333333333333333703, 0.3079598441704289313, 0.3333333333333333703, 0.3079598441704289313, 0.3333333333333333703, 0.3079598441704289313, 0.3333333333333333703, 0.3079598441704289313, 0.3333333333333333703, 0.3079598441704289313, 0.3333333333333333703, 0.3079598441704289313, 0.3333333333333333703, 0.3079598441704289313, 0.3333333333333333703, 0.3079598441704289313, 0.3333333333333333703, 0.3079598441704289313, 0.3333333333333333703, 0.3079598441704289313, 0.3333333333333333703, 0.3079598441704289313, 0.3333333333333333703, 0.3079598441704289313, 0.3333333333333333703, 0.3079598441704289313, 0.3333333333333333703, 0.3079598441704289313, 0.3333333333333333703, 0.3079598441704289313, 0.3333333333333333703),
 ( 0.3333333333333333703, 0.3079598441704289313, 0.3333333333333333703, 0.3079598441704289313, 0.3333333333333333703, 0.3079598441704289313, 0.3333333333333333703, 0.3079598441704289313, 0.3333333333333333703, 0.3079598441704289313, 0.3333333333333333703, 0.3079598441704289313, 0.3333333333333333703, 0.3079598441704289313, 0.3333333333333333703, 0.3079598441704289313, 0.3333333333333333703, 0.3079598441704289313, 0.3333333333333333703, 0.3079598441704289313, 0.3333333333333333703, 0.3079598441704289313, 0.3333333333333333703, 0.3079598441704289313, 0.3333333333333333703, 0.3079598441704289313, 0.3333333333333333703, 0.3079598441704289313, 0.3333333333333333703, 0.3079598441704289313, 0.3333333333333333703, 0.3079598441704289313, 0.3333333333333333703, 0.3079598441704289313, 0.3333333333333333703, 0.3079598441704289313, 0.3333333333333333703, 0.3079598441704289313, 0.3333333333333333703, 0.3079598441704289313, 0.3333333333333333703, 0.3079598441704289313, 0.3333333333333333703, 0.3079598441704289313, 0.3333333333333333703, 0.3079598441704289313, 0.3333333333333333703, 0.3079598441704289313, 0.3333333333333333703, 0.3079598441704289313, 0.3333333333333333703, 0.3079598441704289313, 0.3333333333333333703, 0.3079598441704289313, 0.3333333333333333703, 0.3079598441704289313, 0.3333333333333333703, 0.3079598441704289313, 0.3333333333333333703, 0.3079598441704289313, 0.3333333333333333703, 0.3079598441704289313, 0.3333333333333333703, 0.3079598441704289313, 0.3333333333333333703, 0.3079598441704289313, 0.3333333333333333703, 0.3079598441704289313, 0.3333333333333333703, 0.3079598441704289313, 0.3333333333333333703, 0.3079598441704289313, 0.3333333333333333703, 0.3079598441704289313, 0.3333333333333333703, 0.3079598441704289313, 0.3333333333333333703, 0.3079598441704289313, 0.3333333333333333703, 0.3079598441704289313, 0.3333333333333333703, 0.3079598441704289313, 0.3333333333333333703, 0.3079598441704289313, 0.3333333333333333703, 0.3079598441704289313, 0.3333333333333333703, 0.3079598441704289313, 0.3333333333333333703, 0.3079598441704289313, 0.3333333333333333703, 0.3079598441704289313, 0.3333333333333333703, 0.3079598441704289313, 0.3333333333333333703, 0.3079598441704289313, 0.3333333333333333703),
 ( 1.000000000000000000, 0.9238795325112867385, 1.000000000000000000, 0.9238795325112867385, 1.000000000000000000, 0.9238795325112867385, 1.000000000000000000, 0.9238795325112867385, 1.000000000000000000, 0.9238795325112867385, 1.000000000000000000, 0.9238795325112867385, 1.000000000000000000, 0.9238795325112867385, 1.000000000000000000, 0.9238795325112867385, 1.000000000000000000, 0.9238795325112867385, 1.000000000000000000, 0.9238795325112867385, 1.000000000000000000, 0.9238795325112867385, 1.000000000000000000, 0.9238795325112867385, 1.000000000000000000, 0.9238795325112867385, 1.000000000000000000, 0.9238795325112867385, 1.000000000000000000, 0.9238795325112867385, 1.000000000000000000, 0.9238795325112867385, 1.000000000000000000, 0.9238795325112867385, 1.000000000000000000, 0.9238795325112867385, 1.000000000000000000, 0.9238795325112867385, 1.000000000000000000, 0.9238795325112867385, 1.000000000000000000, 0.9238795325112867385, 1.000000000000000000, 0.9238795325112867385, 1.000000000000000000, 0.9238795325112867385, 1.000000000000000000, 0.9238795325112867385, 1.000000000000000000, 0.9238795325112867385, 1.000000000000000000, 0.9238795325112867385, 1.000000000000000000, 0.9238795325112867385, 1.000000000000000000, 0.9238795325112867385, 1.000000000000000000, 0.9238795325112867385, 1.000000000000000000, 0.9238795325112867385, 1.000000000000000000, 0.9238795325112867385, 1.000000000000000000, 0.9238795325112867385, 1.000000000000000000, 0.9238795325112867385, 1.000000000000000000, 0.9238795325112867385, 1.000000000000000000, 0.9238795325112867385, 1.000000000000000000, 0.9238795325112867385, 1.000000000000000000, 0.9238795325112867385, 1.000000000000000000, 0.9238795325112867385, 1.000000000000000000, 0.9238795325112867385, 1.000000000000000000, 0.9238795325112867385, 1.000000000000000000, 0.9238795325112867385, 1.000000000000000000, 0.9238795325112867385, 1.000000000000000000, 0.9238795325112867385, 1.000000000000000000, 0.9238795325112867385, 1.000000000000000000, 0.9238795325112867385, 1.000000000000000000, 0.9238795325112867385, 1.000000000000000000, 0.9238795325112867385, 1.000000000000000000, 0.9238795325112867385, 1.000000000000000000) ) ) 
 REPRESENTATION_ITEM ( '' )  SURFACE ( )  );
#21064 = EDGE_LOOP ( 'NONE', ( #11304, #7704, #10830 ) ) ;
#21065 = CARTESIAN_POINT ( 'NONE',  ( -3.999999999999999112, 1.656854249492380582, 16.06250000273119838 ) ) ;
#21066 = ORIENTED_EDGE ( 'NONE', *, *, #1176, .F. ) ;
#21067 = CARTESIAN_POINT ( 'NONE',  ( -68.45000000109247651, 7.933012699999995476, 14.99999999999999645 ) ) ;
#21068 = ITEM_DEFINED_TRANSFORMATION ( 'NONE', 'NONE', #17944,  #7318 ) ;
#21069 = EDGE_CURVE ( 'NONE', #20008, #16796, #18546, .T. ) ;
#21070 = EDGE_LOOP ( 'NONE', ( #20694, #16497, #2455, #9632, #16128, #10199 ) ) ;
#21071 = DIRECTION ( 'NONE',  ( -0.5000000000000013323, -0.000000000000000000, -0.8660254037844380415 ) ) ;
#21072 = VERTEX_POINT ( 'NONE', #18670 ) ;
#21073 = EDGE_CURVE ( 'NONE', #22517, #7647, #11274, .T. ) ;
#21074 =( REPRESENTATION_RELATIONSHIP ('NONE','NONE', #8403, #10226 ) REPRESENTATION_RELATIONSHIP_WITH_TRANSFORMATION ( #15834 )SHAPE_REPRESENTATION_RELATIONSHIP( ) );
#21075 = VERTEX_POINT ( 'NONE', #16415 ) ;
#21076 = CARTESIAN_POINT ( 'NONE',  ( -3.458734124999998993, -1.432654583217642497, 11.75000000136560629 ) ) ;
#21077 = CARTESIAN_POINT ( 'NONE',  ( -2.449293598294706907E-16, 4.000000000000000000, -0.8249999972688125682 ) ) ;
#21078 = DIRECTION ( 'NONE',  ( 0.000000000000000000, 0.000000000000000000, 1.000000000000000000 ) ) ;
#21079 = CARTESIAN_POINT ( 'NONE',  ( 67.35000000109248219, 8.538419263543522320, 16.46158073645647235 ) ) ;
#21080 = CARTESIAN_POINT ( 'NONE',  ( -69.95000000000000284, 12.50000000000000000, 16.03553390593273420 ) ) ;
#21081 = CARTESIAN_POINT ( 'NONE',  ( -71.70000000000000284, 9.999999999999998224, 17.49999999999999645 ) ) ;
#21082 = CARTESIAN_POINT ( 'NONE',  ( 53.68518183416157541, 10.06805114094562548, 11.99999999999999645 ) ) ;
#21083 = FACE_BOUND ( 'NONE', #3046, .T. ) ;
#21084 = CARTESIAN_POINT ( 'NONE',  ( -2.117863837641485618E-16, 3.458734125000000770, 0.7375000013655954589 ) ) ;
#21085 = CARTESIAN_POINT ( 'NONE',  ( 2.500000000000000000, 0.000000000000000000, 0.000000000000000000 ) ) ;
#21086 = DIRECTION ( 'NONE',  ( -1.000000000000000000, -0.000000000000000000, -0.000000000000000000 ) ) ;
#21087 = CARTESIAN_POINT ( 'NONE',  ( 4.000000000000001776, -1.656854249492379694, 13.56250000273119660 ) ) ;
#21088 = CARTESIAN_POINT ( 'NONE',  ( 72.50000000000000000, 9.999999999999998224, 14.99999999999999645 ) ) ;
#21089 = ORIENTED_EDGE ( 'NONE', *, *, #21361, .F. ) ;
#21090 = DIRECTION ( 'NONE',  ( 1.000000000000000000, 0.000000000000000000, 0.000000000000000000 ) ) ;
#21091 = ORIENTED_EDGE ( 'NONE', *, *, #8067, .T. ) ;
#21092 = CARTESIAN_POINT ( 'NONE',  ( 58.56018183416157541, 5.999999999999996447, 14.93194885905437808 ) ) ;
#21093 = ADVANCED_FACE ( 'NONE', ( #9467 ), #10923, .T. ) ;
#21094 = EDGE_CURVE ( 'NONE', #13926, #12919, #12837, .T. ) ;
#21095 = CARTESIAN_POINT ( 'NONE',  ( -2.445694354108820523, 2.445694354108820523, 1.612500001365596125 ) ) ;
#21096 = ORIENTED_EDGE ( 'NONE', *, *, #14943, .T. ) ;
#21097 = DIRECTION ( 'NONE',  ( 0.000000000000000000, 8.881784197001252323E-16, 1.000000000000000000 ) ) ;
#21098 = ADVANCED_FACE ( 'NONE', ( #21894 ), #18202, .F. ) ;
#21099 = VERTEX_POINT ( 'NONE', #4059 ) ;
#21100 = VERTEX_POINT ( 'NONE', #13075 ) ;
#21101 = CARTESIAN_POINT ( 'NONE',  ( 55.34606816583843880, 8.825410453826357582, 18.02818770551464667 ) ) ;
#21102 = CARTESIAN_POINT ( 'NONE',  ( -67.65000000218496723, 12.50000000000000000, 16.03553390593273420 ) ) ;
#21103 = CARTESIAN_POINT ( 'NONE',  ( -1.432654583217641164, -3.458734125000000326, -2.824999998634404541 ) ) ;
#21104 = LINE ( 'NONE', #10254, #14129 ) ;
#21105 = CARTESIAN_POINT ( 'NONE',  ( -3.458734124999999437, 1.432654583217640498, 19.62500000136560629 ) ) ;
#21106 = CARTESIAN_POINT ( 'NONE',  ( 4.000000000000000888, 4.898587196589412829E-16, 14.62500000273119660 ) ) ;
#21107 = CARTESIAN_POINT ( 'NONE',  ( 59.53125000000000000, 11.24264068711929276, 18.00000000000000355 ) ) ;
#21108 = CARTESIAN_POINT ( 'NONE',  ( 69.75000000109247367, 8.538419263543522320, 16.46158073645647235 ) ) ;
#21109 = CARTESIAN_POINT ( 'NONE',  ( -4.197393957002303999, 0.4069871074557429025, -3.503767560748926257 ) ) ;
#21110 = CARTESIAN_POINT ( 'NONE',  ( 54.31481816583844591, 12.99999999999999822, 14.93194885905435676 ) ) ;
#21111 = CARTESIAN_POINT ( 'NONE',  ( -3.458734125000000770, 1.432654583217640498, -0.07499999863440427739 ) ) ;
#21112 = CARTESIAN_POINT ( 'NONE',  ( 67.75000000218496155, 11.03553390593276617, 17.49999999999997513 ) ) ;
#21113 = DIRECTION ( 'NONE',  ( 0.000000000000000000, 0.000000000000000000, 1.000000000000000000 ) ) ;
#21114 = VECTOR ( 'NONE', #21311, 1000.000000000000000 ) ;
#21115 = CARTESIAN_POINT ( 'NONE',  ( -68.95000000109247651, 11.46158073645647235, 16.46158073645647235 ) ) ;
#21116 = EDGE_LOOP ( 'NONE', ( #13212, #14581, #6202, #19242 ) ) ;
#21117 = CARTESIAN_POINT ( 'NONE',  ( -20.00005080000000035, 0.000000000000000000, 1.000000000000000000 ) ) ;
#21118 = CARTESIAN_POINT ( 'NONE',  ( 1.656854249492380138, 4.000000000000000000, -2.012499999999998401 ) ) ;
#21119 = VERTEX_POINT ( 'NONE', #7328 ) ;
#21120 = FACE_OUTER_BOUND ( 'NONE', #13773, .T. ) ;
#21121 = SHAPE_REPRESENTATION_RELATIONSHIP ( 'NONE' , 'NONE' ,  #18175, #449 ) ;
#21122 = EDGE_CURVE ( 'NONE', #6430, #15019, #2012, .T. ) ;
#21123 = CARTESIAN_POINT ( 'NONE',  ( -2.828427124746190291, 2.828427124746190291, 2.300000002731188431 ) ) ;
#21124 = VERTEX_POINT ( 'NONE', #2132 ) ;
#21125 = B_SPLINE_CURVE_WITH_KNOTS ( 'NONE', 3,
 ( #11374, #5487, #14853, #16398, #22108, #5728, #21765, #14501, #13060, #4044, #12822, #18652, #7658, #14981, #2241, #7186, #20315, #13169, #16285, #20080, #3680 ),
 .UNSPECIFIED., .F., .F.,
 ( 4, 2, 2, 2, 2, 2, 1, 2, 2, 2, 4 ),
 ( 0.000000000000000000, 0.0009109962461224923582, 0.001821992492244984066, 0.002732988738367476099, 0.003643984984489967698, 0.004099483107551214582, 0.004554981230612460165, 0.005010479353673706615, 0.005465977476734953065, 0.006376973722857446833, 0.007287969968979940601 ),
 .UNSPECIFIED. ) ;
#21126 = ORIENTED_EDGE ( 'NONE', *, *, #11102, .T. ) ;
#21127 = CARTESIAN_POINT ( 'NONE',  ( 7.347880794884118750E-16, -4.000000000000000000, 1.675000002731187987 ) ) ;
#21128 = DIRECTION ( 'NONE',  ( 1.000000000000000000, 0.000000000000000000, -0.000000000000000000 ) ) ;
#21129 = ORIENTED_EDGE ( 'NONE', *, *, #21216, .F. ) ;
#21130 = SURFACE_SIDE_STYLE ('',( #12428 ) ) ;
#21131 = CARTESIAN_POINT ( 'NONE',  ( 67.15000000109247935, 11.46158073645647235, 16.46158073645647235 ) ) ;
#21132 = EDGE_CURVE ( 'NONE', #14572, #11205, #7437, .T. ) ;
#21133 = CARTESIAN_POINT ( 'NONE',  ( 69.55000000109247082, 11.46158073645647235, 13.53841926354352232 ) ) ;
#21134 = AXIS2_PLACEMENT_3D ( 'NONE', #1706, #4969, #10623 ) ;
#21135 = EDGE_LOOP ( 'NONE', ( #16829, #8347, #1896, #15613 ) ) ;
#21136 = DIRECTION ( 'NONE',  ( -0.000000000000000000, -0.000000000000000000, 1.000000000000000000 ) ) ;
#21137 = CARTESIAN_POINT ( 'NONE',  ( 53.43750000000000711, 10.00000000000001776, 18.99999999999999645 ) ) ;
#21138 = CARTESIAN_POINT ( 'NONE',  ( -1.432654583217640276, 3.458734125000000326, 2.550000001365598123 ) ) ;
#21139 = CARTESIAN_POINT ( 'NONE',  ( 1.432654583217641164, 3.458734125000000326, 17.12500000136560629 ) ) ;
#21140 = CARTESIAN_POINT ( 'NONE',  ( -10.00000000000000000, 0.000000000000000000, 0.000000000000000000 ) ) ;
#21141 = CYLINDRICAL_SURFACE ( 'NONE', #11674, 8.749000000000002331 ) ;
#21142 = ORIENTED_EDGE ( 'NONE', *, *, #6567, .F. ) ;
#21143 = FACE_OUTER_BOUND ( 'NONE', #19603, .T. ) ;
#21144 = DIRECTION ( 'NONE',  ( 0.000000000000000000, 0.000000000000000000, -1.000000000000000000 ) ) ;
#21145 = DIRECTION ( 'NONE',  ( 0.000000000000000000, 0.000000000000000000, 1.000000000000000000 ) ) ;
#21146 = ORIENTED_EDGE ( 'NONE', *, *, #22504, .F. ) ;
#21147 = DIRECTION ( 'NONE',  ( 0.000000000000000000, 0.000000000000000000, 1.000000000000000000 ) ) ;
#21148 = CARTESIAN_POINT ( 'NONE',  ( 71.65000000109247935, 9.999999999999998224, 12.93301269999999192 ) ) ;
#21149 = CIRCLE ( 'NONE', #10515, 2.100000000000000089 ) ;
#21150 = DIRECTION ( 'NONE',  ( 0.000000000000000000, 0.000000000000000000, -1.000000000000000000 ) ) ;
#21151 = ORIENTED_EDGE ( 'NONE', *, *, #3484, .F. ) ;
#21152 = DIRECTION ( 'NONE',  ( -1.000000000000000000, 0.000000000000000000, 0.000000000000000000 ) ) ;
#21153 = ORIENTED_EDGE ( 'NONE', *, *, #13905, .F. ) ;
#21154 = CARTESIAN_POINT ( 'NONE',  ( -3.999999999999999112, 1.656854249492380582, 17.93750000000001421 ) ) ;
#21155 = CARTESIAN_POINT ( 'NONE',  ( 70.30000000218494449, 8.232233047033627571, 16.76776695296636532 ) ) ;
#21156 = EDGE_CURVE ( 'NONE', #15687, #7993, #8008, .T. ) ;
#21157 = LINE ( 'NONE', #21270, #16818 ) ;
#21158 =( BOUNDED_CURVE ( )  B_SPLINE_CURVE ( 2, ( #17230, #2361, #9692, #11736, #4638, #22713, #8135, #11972, #16989 ),
 .UNSPECIFIED., .F., .F. ) 
 B_SPLINE_CURVE_WITH_KNOTS ( ( 3, 2, 2, 2, 3 ),
 ( 0.000000000000000000, 0.01562499999999990459, 0.03124999999999980918, 0.04687499999999971551, 0.06249999999999961836 ),
 .UNSPECIFIED. ) 
 CURVE ( )  GEOMETRIC_REPRESENTATION_ITEM ( )  RATIONAL_B_SPLINE_CURVE ( ( 1.000000000000000000, 0.9238795325112867385, 1.000000000000000000, 0.9238795325112867385, 1.000000000000000000, 0.9238795325112867385, 1.000000000000000000, 0.9238795325112886259, 0.9999999999999981126 ) ) 
 REPRESENTATION_ITEM ( '' )  );
#21159 = CARTESIAN_POINT ( 'NONE',  ( 0.000000000000000000, 0.000000000000000000, 0.000000000000000000 ) ) ;
#21160 = CARTESIAN_POINT ( 'NONE',  ( 68.85000000109246798, 12.06698730000000097, 14.99999999999999645 ) ) ;
#21161 = ORIENTED_EDGE ( 'NONE', *, *, #7503, .T. ) ;
#21162 = FACE_OUTER_BOUND ( 'NONE', #3790, .T. ) ;
#21163 = DIRECTION ( 'NONE',  ( 0.000000000000000000, 0.000000000000000000, 1.000000000000000000 ) ) ;
#21164 = EDGE_CURVE ( 'NONE', #21943, #7467, #3844, .T. ) ;
#21165 = CARTESIAN_POINT ( 'NONE',  ( 69.65000000109246514, 12.06698730000000097, 14.99999999999999645 ) ) ;
#21166 = CARTESIAN_POINT ( 'NONE',  ( -3.458734124999998993, 0.000000000000000000, 11.43750000136560452 ) ) ;
#21167 = DIRECTION ( 'NONE',  ( 0.000000000000000000, 0.000000000000000000, 1.000000000000000000 ) ) ;
#21168 = DIRECTION ( 'NONE',  ( 1.000000000000000000, 0.000000000000000000, 0.000000000000000000 ) ) ;
#21169 = EDGE_LOOP ( 'NONE', ( #6303, #10191, #2647, #14092 ) ) ;
#21170 = CARTESIAN_POINT ( 'NONE',  ( 1.656854249492380360, 4.000000000000000000, -1.012499999999997513 ) ) ;
#21171 = CARTESIAN_POINT ( 'NONE',  ( 4.000000000000000888, 4.898587196589412829E-16, 15.50000000000001066 ) ) ;
#21172 = LINE ( 'NONE', #10571, #12022 ) ;
#21173 = CARTESIAN_POINT ( 'NONE',  ( -1.656854249492380582, 4.000000000000000000, -0.8874999999999971800 ) ) ;
#21174 = ORIENTED_EDGE ( 'NONE', *, *, #21466, .T. ) ;
#21175 = CARTESIAN_POINT ( 'NONE',  ( 1.971781867644420635E-15, -4.000000000000000000, 13.37500000273119660 ) ) ;
#21176 = ORIENTED_EDGE ( 'NONE', *, *, #9670, .F. ) ;
#21177 = CARTESIAN_POINT ( 'NONE',  ( -69.15000000109246514, 8.538419263543522320, 16.46158073645647235 ) ) ;
#21178 = ORIENTED_EDGE ( 'NONE', *, *, #10668, .T. ) ;
#21179 = DIRECTION ( 'NONE',  ( 7.087422195345011518E-32, 1.000000000000000000, -0.000000000000000000 ) ) ;
#21180 = ORIENTED_EDGE ( 'NONE', *, *, #2574, .T. ) ;
#21181 = ORIENTED_EDGE ( 'NONE', *, *, #20614, .F. ) ;
#21182 = CARTESIAN_POINT ( 'NONE',  ( 1.432654583217643163, -3.458734124999999882, 13.00000000136560629 ) ) ;
#21183 = DIRECTION ( 'NONE',  ( -0.000000000000000000, -1.000000000000000000, 0.000000000000000000 ) ) ;
#21184 = EDGE_CURVE ( 'NONE', #7010, #8065, #13722, .T. ) ;
#21185 = CARTESIAN_POINT ( 'NONE',  ( -68.10000000218495586, 8.232233047033629347, 13.23223304703362402 ) ) ;
#21186 = EDGE_CURVE ( 'NONE', #12453, #20172, #6097, .T. ) ;
#21187 = DIRECTION ( 'NONE',  ( 0.000000000000000000, -1.000000000000000000, 0.000000000000000000 ) ) ;
#21188 = AXIS2_PLACEMENT_3D ( 'NONE', #18953, #19300, #12037 ) ;
#21189 = CARTESIAN_POINT ( 'NONE',  ( -69.59999999999999432, 8.232233047033629347, 13.23223304703362402 ) ) ;
#21190 = AXIS2_PLACEMENT_3D ( 'NONE', #19378, #4779, #19617 ) ;
#21191 = CARTESIAN_POINT ( 'NONE',  ( -71.45000000000000284, 12.50000000000000000, 13.96446609406725692 ) ) ;
#21192 = EDGE_CURVE ( 'NONE', #10634, #12600, #4691, .T. ) ;
#21193 = CARTESIAN_POINT ( 'NONE',  ( 60.00000000000005684, 13.04144815258546330, 15.11939319870875309 ) ) ;
#21194 = EDGE_CURVE ( 'NONE', #4306, #21201, #10704, .T. ) ;
#21195 =( BOUNDED_CURVE ( )  B_SPLINE_CURVE ( 2, ( #9109, #7425, #14735, #5608, #2589, #18889, #17100, #8367, #13413 ),
 .UNSPECIFIED., .F., .F. ) 
 B_SPLINE_CURVE_WITH_KNOTS ( ( 3, 2, 2, 2, 3 ),
 ( 0.7499999999999997780, 0.7656249999999996669, 0.7812499999999995559, 0.7968749999999994449, 0.8124999999999993339 ),
 .UNSPECIFIED. ) 
 CURVE ( )  GEOMETRIC_REPRESENTATION_ITEM ( )  RATIONAL_B_SPLINE_CURVE ( ( 1.000000000000001110, 0.9238795325112856283, 1.000000000000000000, 0.9238795325112867385, 1.000000000000000000, 0.9238795325112867385, 1.000000000000000000, 0.9238795325112899581, 0.9999999999999967804 ) ) 
 REPRESENTATION_ITEM ( '' )  );
#21196 = CARTESIAN_POINT ( 'NONE',  ( 3.458734125000001214, -1.432654583217639610, -1.574999998634403875 ) ) ;
#21197 = CARTESIAN_POINT ( 'NONE',  ( -3.999999999999998224, -1.656854249492383024, 13.06250000000001243 ) ) ;
#21198 = DIRECTION ( 'NONE',  ( 0.000000000000000000, 0.000000000000000000, 1.000000000000000000 ) ) ;
#21199 = CARTESIAN_POINT ( 'NONE',  ( 4.000000000000001776, -1.656854249492379694, 11.56250000273119838 ) ) ;
#21200 = DIRECTION ( 'NONE',  ( -0.000000000000000000, -0.000000000000000000, 1.000000000000000000 ) ) ;
#21201 = VERTEX_POINT ( 'NONE', #13303 ) ;
#21202 = CARTESIAN_POINT ( 'NONE',  ( -71.75000000109248788, 11.46158073645647235, 13.53841926354352232 ) ) ;
#21203 = ORIENTED_EDGE ( 'NONE', *, *, #18424, .F. ) ;
#21204 = CARTESIAN_POINT ( 'NONE',  ( 54.34143183416158251, 8.689308171935088865, 17.97181229448535689 ) ) ;
#21205 = CARTESIAN_POINT ( 'NONE',  ( -69.95000000109247651, 8.538419263543524096, 13.53841926354352054 ) ) ;
#21206 = CARTESIAN_POINT ( 'NONE',  ( -1.432654583217640942, -3.458734124999999882, 1.925000001365597457 ) ) ;
#21207 = VERTEX_POINT ( 'NONE', #9709 ) ;
#21208 = CARTESIAN_POINT ( 'NONE',  ( -11.83859044676619199, -9.000000000000003553, 10.00000000000008882 ) ) ;
#21209 = AXIS2_PLACEMENT_3D ( 'NONE', #22005, #20326, #3470 ) ;
#21210 = ORIENTED_EDGE ( 'NONE', *, *, #2932, .F. ) ;
#21211 = VECTOR ( 'NONE', #5967, 1000.000000000000000 ) ;
#21212 = CARTESIAN_POINT ( 'NONE',  ( 5.577176569667260608, -11.25000000000000355, 5.000000000000079936 ) ) ;
#21213 = ORIENTED_EDGE ( 'NONE', *, *, #13484, .F. ) ;
#21214 = CARTESIAN_POINT ( 'NONE',  ( 51.03356816583844591, 11.72490539043803004, 18.97181229448534268 ) ) ;
#21215 = CARTESIAN_POINT ( 'NONE',  ( -66.15000000218495302, 11.03553390593273598, 17.50000000000000355 ) ) ;
#21216 = EDGE_CURVE ( 'NONE', #18117, #11987, #13431, .T. ) ;
#21217 = CARTESIAN_POINT ( 'NONE',  ( 4.999999999999999112, 9.314797388894909602, -1.239665997526783858 ) ) ;
#21218 = DIRECTION ( 'NONE',  ( 0.000000000000000000, 0.000000000000000000, -1.000000000000000000 ) ) ;
#21219 = CARTESIAN_POINT ( 'NONE',  ( 1.025207404391860050E-15, 3.458734125000000770, 15.43750000136560452 ) ) ;
#21220 = CARTESIAN_POINT ( 'NONE',  ( -3.999999999999998224, -1.656854249492383246, 14.18750000273119483 ) ) ;
#21221 = CARTESIAN_POINT ( 'NONE',  ( 57.37500000000000000, 7.878679656440349177, 12.87867965644035984 ) ) ;
#21222 = CARTESIAN_POINT ( 'NONE',  ( 68.25000000109247367, 7.933012699999995476, 14.99999999999999645 ) ) ;
#21223 = ADVANCED_FACE ( 'NONE', ( #9826 ), #20695, .T. ) ;
#21225 = CARTESIAN_POINT ( 'NONE',  ( 60.00000000000000711, 12.12132034355963484, 12.87867965644034740 ) ) ;
#21224 = VECTOR ( 'NONE', #5175, 1000.000000000000000 ) ;
#21226 = CARTESIAN_POINT ( 'NONE',  ( 57.46875000000000711, 6.999999999999992895, 13.75735931288071967 ) ) ;
#21227 = AXIS2_PLACEMENT_3D ( 'NONE', #20531, #16849, #22081 ) ;
#21228 = CARTESIAN_POINT ( 'NONE',  ( -3.458734125000000326, -1.432654583217642497, 3.050000001365598568 ) ) ;
#21229 = CARTESIAN_POINT ( 'NONE',  ( 67.60000000218495586, 12.50000000000000000, 14.99999999999999645 ) ) ;
#21230 = CARTESIAN_POINT ( 'NONE',  ( 4.688305830332750723, -11.25000000000000355, 10.00000000000008882 ) ) ;
#21231 = CARTESIAN_POINT ( 'NONE',  ( -69.30000000109247082, 7.933012699999995476, 14.14382582708705094 ) ) ;
#21232 = VERTEX_POINT ( 'NONE', #2730 ) ;
#21233 = CARTESIAN_POINT ( 'NONE',  ( 4.999999999999999112, 0.4999240074894452657, 8.734705317681628500 ) ) ;
#21234 = LINE ( 'NONE', #5322, #3614 ) ;
#21235 = VERTEX_POINT ( 'NONE', #18796 ) ;
#21236 = CARTESIAN_POINT ( 'NONE',  ( -2.828427124746188515, -2.828427124746190735, 15.25000000273119660 ) ) ;
#21237 = CARTESIAN_POINT ( 'NONE',  ( 4.000000000000000000, 4.898587196589412829E-16, 0.9250000027311873207 ) ) ;
#21238 = ORIENTED_EDGE ( 'NONE', *, *, #18327, .T. ) ;
#21239 = ORIENTED_EDGE ( 'NONE', *, *, #6702, .T. ) ;
#21240 = CIRCLE ( 'NONE', #3656, 10.00000000000000178 ) ;
#21241 = CARTESIAN_POINT ( 'NONE',  ( 2.697128823393878605, -5.948365447239590154, -0.01372220897662065377 ) ) ;
#21242 = DIRECTION ( 'NONE',  ( 1.000000000000000000, 7.703719777548943412E-32, 0.000000000000000000 ) ) ;
#21243 = ORIENTED_EDGE ( 'NONE', *, *, #10275, .F. ) ;
#21244 = LINE ( 'NONE', #21481, #10709 ) ;
#21245 = UNCERTAINTY_MEASURE_WITH_UNIT (LENGTH_MEASURE( 1.000000000000000082E-05 ), #21286, 'distance_accuracy_value', 'NONE');
#21246 = CARTESIAN_POINT ( 'NONE',  ( 4.999999999999999112, 6.772677083992387992, 5.538577986808924436 ) ) ;
#21247 = CARTESIAN_POINT ( 'NONE',  ( 69.05000000109247082, 9.999999999999998224, 17.06698730000000097 ) ) ;
#21248 = EDGE_CURVE ( 'NONE', #13749, #3286, #2489, .T. ) ;
#21249 = EDGE_LOOP ( 'NONE', ( #11025, #14327, #11341, #16501 ) ) ;
#21250 = CARTESIAN_POINT ( 'NONE',  ( 2.500000000000000000, 1.178949249685212974, -2.042000000000001148 ) ) ;
#21251 = CARTESIAN_POINT ( 'NONE',  ( 52.03124999999999289, 11.65685424949239923, 18.99999999999998934 ) ) ;
#21252 = CARTESIAN_POINT ( 'NONE',  ( 2.445694354108820523, -2.445694354108820079, 4.112500001365594571 ) ) ;
#21253 = CARTESIAN_POINT ( 'NONE',  ( 1.872352939448454495E-15, -3.458734125000000326, 14.68750000136560452 ) ) ;
#21254 = DIRECTION ( 'NONE',  ( -0.000000000000000000, -1.000000000000000000, -0.000000000000000000 ) ) ;
#21255 = FACE_OUTER_BOUND ( 'NONE', #4179, .T. ) ;
#21256 = EDGE_LOOP ( 'NONE', ( #10404, #16328, #9588, #1802 ) ) ;
#21257 = DIRECTION ( 'NONE',  ( 1.000000000000000000, 7.703719777548943412E-32, 0.000000000000000000 ) ) ;
#21258 = DIRECTION ( 'NONE',  ( 0.000000000000000000, -0.000000000000000000, 1.000000000000000000 ) ) ;
#21259 = CARTESIAN_POINT ( 'NONE',  ( 2.828427124746190735, -2.828427124746189847, -1.324999999999997957 ) ) ;
#21260 = VERTEX_POINT ( 'NONE', #578 ) ;
#21261 = DIRECTION ( 'NONE',  ( 0.3420201433256622181, 0.9396926207859107594, -6.162975822039141593E-32 ) ) ;
#21262 = CARTESIAN_POINT ( 'NONE',  ( 72.00000000109248788, 10.85617417291294551, 17.06698729999999742 ) ) ;
#21263 = CARTESIAN_POINT ( 'NONE',  ( 0.000000000000000000, 0.000000000000000000, 0.000000000000000000 ) ) ;
#21264 = ORIENTED_EDGE ( 'NONE', *, *, #19180, .F. ) ;
#21265 = CARTESIAN_POINT ( 'NONE',  ( -69.54999999999999716, 7.499999999999996447, 13.96446609406725514 ) ) ;
#21266 = ORIENTED_EDGE ( 'NONE', *, *, #3000, .F. ) ;
#21267 = CARTESIAN_POINT ( 'NONE',  ( 52.59375000000000711, 11.65685424949236193, 10.99999999999998401 ) ) ;
#21268 = CARTESIAN_POINT ( 'NONE',  ( 71.30000000218494449, 8.232233047033629347, 13.23223304703362402 ) ) ;
#21269 = VECTOR ( 'NONE', #10506, 1000.000000000000114 ) ;
#21270 = CARTESIAN_POINT ( 'NONE',  ( 30.70991776966726405, -11.25000000000000355, 5.000000000000079936 ) ) ;
#21271 = CARTESIAN_POINT ( 'NONE',  ( 14.99999999999995737, -15.00000000000000000, -50.00000000000000000 ) ) ;
#21272 = CARTESIAN_POINT ( 'NONE',  ( 67.60000000109246798, 7.933012699999995476, 15.85617417291294196 ) ) ;
#21273 = ORIENTED_EDGE ( 'NONE', *, *, #10428, .F. ) ;
#21274 = CARTESIAN_POINT ( 'NONE',  ( -68.60000000218495586, 9.999999999999998224, 17.49999999999999645 ) ) ;
#21275 = DIRECTION ( 'NONE',  ( 0.000000000000000000, 0.000000000000000000, 1.000000000000000000 ) ) ;
#21276 = DIRECTION ( 'NONE',  ( -1.000000000000000000, -0.000000000000000000, -0.000000000000000000 ) ) ;
#21277 = AXIS2_PLACEMENT_3D ( 'NONE', #15430, #2567, #9675 ) ;
#21278 = CARTESIAN_POINT ( 'NONE',  ( -3.458734124999998993, -1.432654583217642497, 10.50000000136560452 ) ) ;
#21279 = CARTESIAN_POINT ( 'NONE',  ( 4.999999999999999112, -2.223716399045630343, 8.461683424509308438 ) ) ;
#21280 = AXIS2_PLACEMENT_3D ( 'NONE', #20397, #19935, #5808 ) ;
#21281 = DIRECTION ( 'NONE',  ( -1.000000000000000000, 0.000000000000000000, 0.000000000000000000 ) ) ;
#21282 = VERTEX_POINT ( 'NONE', #8027 ) ;
#21283 = CARTESIAN_POINT ( 'NONE',  ( -4.000000000000000000, -1.656854249492383246, -1.637499999999997735 ) ) ;
#21284 = CARTESIAN_POINT ( 'NONE',  ( -55.00000000000000000, -15.00000000000000000, 10.00000000000001599 ) ) ;
#21285 = CARTESIAN_POINT ( 'NONE',  ( 66.54999999999999716, 11.03553390593269867, 12.49999999999995559 ) ) ;
#21286 =( LENGTH_UNIT ( ) NAMED_UNIT ( * ) SI_UNIT ( .MILLI., .METRE. ) );
#21287 = ORIENTED_EDGE ( 'NONE', *, *, #10860, .F. ) ;
#21288 = EDGE_CURVE ( 'NONE', #15099, #18435, #15292, .T. ) ;
#21289 = CARTESIAN_POINT ( 'NONE',  ( -3.999999999999998224, -1.656854249492383024, 13.18750000273119660 ) ) ;
#21290 = ORIENTED_EDGE ( 'NONE', *, *, #6472, .T. ) ;
#21291 = CARTESIAN_POINT ( 'NONE',  ( -6.499999999999999112, 2.531211054341939271, -0.2595069192555971571 ) ) ;
#21292 = ORIENTED_EDGE ( 'NONE', *, *, #21248, .T. ) ;
#21293 = DIRECTION ( 'NONE',  ( -1.224646799147353207E-16, 0.000000000000000000, -1.000000000000000000 ) ) ;
#21294 = ORIENTED_EDGE ( 'NONE', *, *, #11725, .F. ) ;
#21295 =( BOUNDED_CURVE ( )  B_SPLINE_CURVE ( 2, ( #21081, #4806, #17402, #9748, #2768, #21191, #19184, #20960, #17518 ),
 .UNSPECIFIED., .F., .F. ) 
 B_SPLINE_CURVE_WITH_KNOTS ( ( 3, 2, 2, 2, 3 ),
 ( 0.1249999999999992367, 0.1406249999999996947, 0.1562500000000001388, 0.1718750000000005829, 0.1875000000000010270 ),
 .UNSPECIFIED. ) 
 CURVE ( )  GEOMETRIC_REPRESENTATION_ITEM ( )  RATIONAL_B_SPLINE_CURVE ( ( 1.000000000000003775, 0.9238795325112830747, 1.000000000000000000, 0.9238795325112867385, 1.000000000000000000, 0.9238795325112867385, 1.000000000000000000, 0.9238795325112817425, 1.000000000000005107 ) ) 
 REPRESENTATION_ITEM ( '' )  );
#21296 = ORIENTED_EDGE ( 'NONE', *, *, #12756, .T. ) ;
#21297 = CARTESIAN_POINT ( 'NONE',  ( 2.445694354108822299, -2.445694354108820079, 12.06250000136560629 ) ) ;
#21298 = ADVANCED_FACE ( 'NONE', ( #694 ), #927, .T. ) ;
#21299 = CARTESIAN_POINT ( 'NONE',  ( 52.12500000000000711, 12.12132034355964727, 17.12132034355963484 ) ) ;
#21300 = COLOUR_RGB ( '', 0.09019608, 0.27058824, 0.51372549) ;
#21301 = CIRCLE ( 'NONE', #7190, 6.760799999999997034 ) ;
#21302 = DIRECTION ( 'NONE',  ( 1.000000000000000000, 0.000000000000000000, 0.000000000000000000 ) ) ;
#21303 = FACE_OUTER_BOUND ( 'NONE', #2679, .T. ) ;
#21304 = CARTESIAN_POINT ( 'NONE',  ( -3.861362476283256129, -2.629030857716004199, -3.671615880910374941 ) ) ;
#21305 = CARTESIAN_POINT ( 'NONE',  ( -68.89999999999999147, 9.999999999999998224, 12.49999999999999289 ) ) ;
#21306 = CARTESIAN_POINT ( 'NONE',  ( -31.74999999999995737, 0.000000000000000000, 0.000000000000000000 ) ) ;
#21307 = CARTESIAN_POINT ( 'NONE',  ( 60.00000000000003553, 13.00089921235714741, 17.44255260030195842 ) ) ;
#21308 = VECTOR ( 'NONE', #11010, 1000.000000000000000 ) ;
#21309 = CARTESIAN_POINT ( 'NONE',  ( -1.432654583217640498, 3.458734125000000770, -1.199999998634403431 ) ) ;
#21310 = CYLINDRICAL_SURFACE ( 'NONE', #10341, 4.000000000000001776 ) ;
#21311 = DIRECTION ( 'NONE',  ( -1.000000000000000000, 0.000000000000000000, 1.982541115402065110E-16 ) ) ;
#21312 = CARTESIAN_POINT ( 'NONE',  ( 2.445694354108821411, 2.445694354108820523, 19.06250000136560629 ) ) ;
#21313 = CARTESIAN_POINT ( 'NONE',  ( 4.203833317240879275, 1.627343821129582979, -3.597273115243889929 ) ) ;
#21314 = VECTOR ( 'NONE', #11581, 999.9999999999997726 ) ;
#21315 = ORIENTED_EDGE ( 'NONE', *, *, #20063, .F. ) ;
#21316 = ADVANCED_FACE ( 'NONE', ( #22616, #22368, #5979, #20808 ), #4415, .T. ) ;
#21317 = CIRCLE ( 'NONE', #17529, 0.03079999999999923077 ) ;
#21318 = DIRECTION ( 'NONE',  ( 0.000000000000000000, 0.000000000000000000, 1.000000000000000000 ) ) ;
#21319 = ORIENTED_EDGE ( 'NONE', *, *, #7323, .F. ) ;
#21320 = CARTESIAN_POINT ( 'NONE',  ( 54.43518183416157541, 9.931948859054372747, 17.99999999999999645 ) ) ;
#21321 = CARTESIAN_POINT ( 'NONE',  ( -66.00000000109247367, 9.143825827087050939, 12.93301269999999370 ) ) ;
#21322 =( LENGTH_UNIT ( ) NAMED_UNIT ( * ) SI_UNIT ( .MILLI., .METRE. ) );
#21323 = EDGE_CURVE ( 'NONE', #22906, #11604, #13373, .T. ) ;
#21324 = CARTESIAN_POINT ( 'NONE',  ( 2.445694354108820523, -2.445694354108820079, -1.887499998634403431 ) ) ;
#21325 = ORIENTED_EDGE ( 'NONE', *, *, #8429, .F. ) ;
#21326 = CARTESIAN_POINT ( 'NONE',  ( 4.999999999999999112, -5.538577986808947529, 6.772677083992368452 ) ) ;
#21327 = VECTOR ( 'NONE', #3621, 1000.000000000000000 ) ;
#21328 = ORIENTED_EDGE ( 'NONE', *, *, #9721, .T. ) ;
#21329 = CARTESIAN_POINT ( 'NONE',  ( 2.828427124746191179, 2.828427124746190291, 19.62500000000001066 ) ) ;
#21330 = ORIENTED_EDGE ( 'NONE', *, *, #13353, .T. ) ;
#21331 = EDGE_CURVE ( 'NONE', #22910, #4760, #20884, .T. ) ;
#21332 = CARTESIAN_POINT ( 'NONE',  ( 50.09606816583843880, 11.58880310854672935, 10.97181229448534445 ) ) ;
#21333 = CIRCLE ( 'NONE', #5283, 8.073750000000021743 ) ;
#21334 = CARTESIAN_POINT ( 'NONE',  ( -66.05000000218494449, 12.50000000000000000, 16.03553390593273420 ) ) ;
#21335 = DIRECTION ( 'NONE',  ( -1.000000000000000000, -0.000000000000000000, -0.000000000000000000 ) ) ;
#21336 = VECTOR ( 'NONE', #10184, 1000.000000000000000 ) ;
#21337 = CARTESIAN_POINT ( 'NONE',  ( -72.25000000109247367, 9.999999999999998224, 17.06698730000000097 ) ) ;
#21338 = VECTOR ( 'NONE', #17004, 1000.000000000000000 ) ;
#21339 = CARTESIAN_POINT ( 'NONE',  ( 3.458734125000001658, 4.235727675282972223E-16, 15.18750000136560452 ) ) ;
#21340 = DIRECTION ( 'NONE',  ( 0.000000000000000000, 0.000000000000000000, 1.000000000000000000 ) ) ;
#21341 = CARTESIAN_POINT ( 'NONE',  ( 0.000000000000000000, 0.000000000000000000, 0.000000000000000000 ) ) ;
#21342 = CARTESIAN_POINT ( 'NONE',  ( 58.68750000000000000, 9.999999999999989342, 11.99999999999999467 ) ) ;
#21343 = EDGE_CURVE ( 'NONE', #11403, #21998, #1275, .T. ) ;
#21344 = CARTESIAN_POINT ( 'NONE',  ( 1.432654583217640276, 3.458734125000000770, 1.675000001365597235 ) ) ;
#21345 = CARTESIAN_POINT ( 'NONE',  ( 1.971781867644420635E-15, -4.000000000000000000, 18.37500000273119483 ) ) ;
#21346 = AXIS2_PLACEMENT_3D ( 'NONE', #6355, #2741, #6473 ) ;
#21347 = SURFACE_SIDE_STYLE ('',( #23157 ) ) ;
#21348 = AXIS2_PLACEMENT_3D ( 'NONE', #10138, #996, #2439 ) ;
#21349 = ORIENTED_EDGE ( 'NONE', *, *, #9854, .F. ) ;
#21350 = DIRECTION ( 'NONE',  ( 1.000000000000000000, 0.000000000000000000, 0.000000000000000000 ) ) ;
#21351 = CARTESIAN_POINT ( 'NONE',  ( -2.000000000000001776, 1.089935651241147118E-15, 8.800000000000022027 ) ) ;
#21352 = ORIENTED_EDGE ( 'NONE', *, *, #19782, .T. ) ;
#21353 = CARTESIAN_POINT ( 'NONE',  ( 59.62500000000000711, 12.12132034355964727, 17.12132034355963484 ) ) ;
#21354 = CARTESIAN_POINT ( 'NONE',  ( -4.000000000000000888, 1.656854249492380804, 1.362500002731187321 ) ) ;
#21355 = EDGE_CURVE ( 'NONE', #7935, #23355, #18590, .T. ) ;
#21356 = ORIENTED_EDGE ( 'NONE', *, *, #20672, .T. ) ;
#21357 = ORIENTED_EDGE ( 'NONE', *, *, #14106, .F. ) ;
#21358 = VECTOR ( 'NONE', #3695, 1000.000000000000114 ) ;
#21359 = CARTESIAN_POINT ( 'NONE',  ( 34.99999999999999289, 4.500000000000001776, -50.00000000000000000 ) ) ;
#21360 = EDGE_LOOP ( 'NONE', ( #20945, #11612, #240, #15080, #155, #11034, #5390, #12156, #1728, #17812, #10723, #12775, #6486, #8417, #20176, #20748 ) ) ;
#21361 = EDGE_CURVE ( 'NONE', #16525, #17599, #3004, .T. ) ;
#21362 = FILL_AREA_STYLE_COLOUR ( '', #11483 ) ;
#21363 = ADVANCED_FACE ( 'NONE', ( #12341 ), #10431, .F. ) ;
#21364 = VECTOR ( 'NONE', #10798, 1000.000000000000000 ) ;
#21365 = FACE_OUTER_BOUND ( 'NONE', #13924, .T. ) ;
#21366 = VERTEX_POINT ( 'NONE', #19602 ) ;
#21367 = CIRCLE ( 'NONE', #336, 2.500000000000000444 ) ;
#21368 = CARTESIAN_POINT ( 'NONE',  ( 4.000000000000000000, 4.898587196589412829E-16, 1.800000000000001155 ) ) ;
#21369 = CIRCLE ( 'NONE', #6498, 2.700000000000000622 ) ;
#21370 = CARTESIAN_POINT ( 'NONE',  ( 66.35000000109246798, 11.46158073645647235, 13.53841926354352232 ) ) ;
#21371 = DIRECTION ( 'NONE',  ( 0.000000000000000000, 0.000000000000000000, 1.000000000000000000 ) ) ;
#21372 = DIRECTION ( 'NONE',  ( 0.3420201433256622181, 0.9396926207859107594, -6.162975822039141593E-32 ) ) ;
#21373 = AXIS2_PLACEMENT_3D ( 'NONE', #9797, #16862, #20543 ) ;
#21374 = CARTESIAN_POINT ( 'NONE',  ( 51.93750000000000711, 10.00000000000001776, 18.99999999999999645 ) ) ;
#21375 = CARTESIAN_POINT ( 'NONE',  ( 2.445694354108820523, -2.445694354108820079, 2.112500001365596791 ) ) ;
#21376 = CARTESIAN_POINT ( 'NONE',  ( 3.458734125000001214, 4.235727675282971730E-16, 12.93750000136560452 ) ) ;
#21377 = CARTESIAN_POINT ( 'NONE',  ( 67.95000000218495018, 7.499999999999996447, 16.03553390593273775 ) ) ;
#21378 = APPLICATION_CONTEXT ( 'automotive_design' ) ;
#21379 = DIRECTION ( 'NONE',  ( -0.000000000000000000, -0.000000000000000000, -1.000000000000000000 ) ) ;
#21380 = ORIENTED_EDGE ( 'NONE', *, *, #2051, .T. ) ;
#21381 = CARTESIAN_POINT ( 'NONE',  ( -1.645496052585941671, 3.496231076593029119, 2.039999999999998259 ) ) ;
#21382 = DIRECTION ( 'NONE',  ( -1.000000000000000000, 0.000000000000000000, -0.000000000000000000 ) ) ;
#21383 = DIRECTION ( 'NONE',  ( -1.060575238724910366E-16, 0.4999999999999951150, -0.8660254037844414832 ) ) ;
#21384 = AXIS2_PLACEMENT_3D ( 'NONE', #12736, #7214, #18090 ) ;
#21385 = EDGE_LOOP ( 'NONE', ( #17958, #18647, #2811, #7329 ) ) ;
#21386 = AXIS2_PLACEMENT_3D ( 'NONE', #15062, #18749, #14821 ) ;
#21387 = PLANE ( 'NONE',  #19067 ) ;
#21388 = CARTESIAN_POINT ( 'NONE',  ( 71.90000000109247935, 12.06698730000000275, 15.85617417291294196 ) ) ;
#21389 = EDGE_CURVE ( 'NONE', #16036, #20854, #21021, .T. ) ;
#21390 = PLANE ( 'NONE',  #15233 ) ;
#21391 = ORIENTED_EDGE ( 'NONE', *, *, #21122, .F. ) ;
#21392 = ORIENTED_EDGE ( 'NONE', *, *, #16152, .F. ) ;
#21393 = AXIS2_PLACEMENT_3D ( 'NONE', #7892, #4289, #2478 ) ;
#21394 = B_SPLINE_CURVE_WITH_KNOTS ( 'NONE', 3,
 ( #21780, #3115, #1299, #8639, #17848, #14516, #23219, #21537 ),
 .UNSPECIFIED., .F., .F.,
 ( 4, 2, 2, 4 ),
 ( 2.465131517071610173E-07, 0.001183067374689837636, 0.001774477805458902699, 0.002365888236227967761 ),
 .UNSPECIFIED. ) ;
#21395 = ADVANCED_FACE ( 'NONE', ( #21631 ), #17823, .T. ) ;
#21396 = CARTESIAN_POINT ( 'NONE',  ( 51.00000000000000711, 12.82842712474617741, 12.17157287525379239 ) ) ;
#21397 = AXIS2_PLACEMENT_3D ( 'NONE', #3044, #17442, #10035 ) ;
#21398 = CARTESIAN_POINT ( 'NONE',  ( 68.45000000218493597, 12.50000000000000000, 16.03553390593273420 ) ) ;
#21399 = LINE ( 'NONE', #22979, #6496 ) ;
#21400 = DIRECTION ( 'NONE',  ( 0.000000000000000000, 0.000000000000000000, 1.000000000000000000 ) ) ;
#21401 = CARTESIAN_POINT ( 'NONE',  ( 67.15000000109247935, 11.46158073645647235, 13.53841926354352232 ) ) ;
#21402 = ORIENTED_EDGE ( 'NONE', *, *, #8370, .T. ) ;
#21403 = DIRECTION ( 'NONE',  ( 0.000000000000000000, -1.000000000000000000, 0.000000000000000000 ) ) ;
#21404 = CARTESIAN_POINT ( 'NONE',  ( 16.43574340323381122, -9.000000000000001776, 5.000000000000079936 ) ) ;
#21405 = CARTESIAN_POINT ( 'NONE',  ( 68.10000000109245377, 12.06698730000000275, 15.85617417291294196 ) ) ;
#21406 = CARTESIAN_POINT ( 'NONE',  ( 1.432654583217643163, -3.458734124999999882, 19.00000000136560629 ) ) ;
#21407 = CIRCLE ( 'NONE', #22571, 2.500000000000002220 ) ;
#21408 = LINE ( 'NONE', #12116, #13978 ) ;
#21409 = CARTESIAN_POINT ( 'NONE',  ( -6.500000000000000000, -3.752776749732572359, -3.700000000000000178 ) ) ;
#21410 = VECTOR ( 'NONE', #18599, 1000.000000000000000 ) ;
#21411 = VERTEX_POINT ( 'NONE', #6936 ) ;
#21412 = CARTESIAN_POINT ( 'NONE',  ( -2.842195834095098572, 1.980645989956865138, -3.295601554149321988 ) ) ;
#21413 = CARTESIAN_POINT ( 'NONE',  ( 58.21875000000000711, 13.00000000000000533, 16.24264068711927322 ) ) ;
#21414 = CARTESIAN_POINT ( 'NONE',  ( -4.000000000000000000, 0.000000000000000000, 0.4250000027311868211 ) ) ;
#21415 =( NAMED_UNIT ( * ) PLANE_ANGLE_UNIT ( ) SI_UNIT ( $, .RADIAN. ) );
#21416 = ORIENTED_EDGE ( 'NONE', *, *, #10164, .T. ) ;
#21417 = DIRECTION ( 'NONE',  ( 0.000000000000000000, 0.000000000000000000, -1.000000000000000000 ) ) ;
#21418 = DIRECTION ( 'NONE',  ( 0.000000000000000000, 0.000000000000000000, -1.000000000000000000 ) ) ;
#21419 = DIRECTION ( 'NONE',  ( 1.000000000000000000, -0.000000000000000000, -0.000000000000000000 ) ) ;
#21420 = ORIENTED_EDGE ( 'NONE', *, *, #14104, .T. ) ;
#21421 = PLANE ( 'NONE',  #6352 ) ;
#21422 = VERTEX_POINT ( 'NONE', #1047 ) ;
#21423 = CARTESIAN_POINT ( 'NONE',  ( 0.000000000000000000, 0.000000000000000000, 0.000000000000000000 ) ) ;
#21424 = VERTEX_POINT ( 'NONE', #22973 ) ;
#21425 = CARTESIAN_POINT ( 'NONE',  ( 2.445694354108821411, 2.445694354108820523, 13.31250000136560452 ) ) ;
#21426 = AXIS2_PLACEMENT_3D ( 'NONE', #18325, #5153, #16309 ) ;
#21427 = LINE ( 'NONE', #8425, #2936 ) ;
#21428 = CARTESIAN_POINT ( 'NONE',  ( 65.90000000109247935, 7.933012699999995476, 14.14382582708705094 ) ) ;
#21429 = CARTESIAN_POINT ( 'NONE',  ( -3.510273485745307287, -2.827716139362669967, -3.610536846335890004 ) ) ;
#21430 = EDGE_CURVE ( 'NONE', #5492, #22748, #23081, .T. ) ;
#21431 = CARTESIAN_POINT ( 'NONE',  ( -69.20000000000000284, 11.76776695296636888, 16.76776695296636532 ) ) ;
#21432 = CARTESIAN_POINT ( 'NONE',  ( 0.000000000000000000, 0.000000000000000000, 9.480888224575631185 ) ) ;
#21433 = CARTESIAN_POINT ( 'NONE',  ( 60.00000000000002132, 11.14543721897689110, 18.43906226982675634 ) ) ;
#21434 = CARTESIAN_POINT ( 'NONE',  ( -2.117863837641485618E-16, 3.458734125000000770, 1.737500001365596347 ) ) ;
#21435 = LINE ( 'NONE', #10594, #3415 ) ;
#21436 = CARTESIAN_POINT ( 'NONE',  ( 34.99999999999999289, 4.500000000000009770, -50.00000000000000711 ) ) ;
#21437 = CARTESIAN_POINT ( 'NONE',  ( -1.432654583217639610, -3.458734124999999882, 15.62500000136560629 ) ) ;
#21438 = FACE_OUTER_BOUND ( 'NONE', #22403, .T. ) ;
#21439 = CIRCLE ( 'NONE', #10406, 4.000000000000001776 ) ;
#21440 = ORIENTED_EDGE ( 'NONE', *, *, #10831, .F. ) ;
#21441 = LINE ( 'NONE', #8666, #17399 ) ;
#21442 = ORIENTED_EDGE ( 'NONE', *, *, #7492, .F. ) ;
#21443 = CARTESIAN_POINT ( 'NONE',  ( 60.34143183416158962, 8.275094609562001935, 18.97181229448536044 ) ) ;
#21444 = CARTESIAN_POINT ( 'NONE',  ( -66.55000000109247082, 8.538419263543522320, 16.46158073645647235 ) ) ;
#21445 = DIRECTION ( 'NONE',  ( 5.551115123125787632E-17, -1.110223024625156540E-16, 1.000000000000000222 ) ) ;
#21446 =( BOUNDED_CURVE ( )  B_SPLINE_CURVE ( 2, ( #13981, #10161, #23169, #8834, #21599, #6902, #19229, #2818, #17456 ),
 .UNSPECIFIED., .F., .F. ) 
 B_SPLINE_CURVE_WITH_KNOTS ( ( 3, 2, 2, 2, 3 ),
 ( 0.8749999999999990008, 0.8906249999999994449, 0.9062499999999998890, 0.9218750000000003331, 0.9375000000000007772 ),
 .UNSPECIFIED. ) 
 CURVE ( )  GEOMETRIC_REPRESENTATION_ITEM ( )  RATIONAL_B_SPLINE_CURVE ( ( 1.000000000000004885, 0.9238795325112818535, 1.000000000000000000, 0.9238795325112867385, 1.000000000000000000, 0.9238795325112867385, 1.000000000000000000, 0.9238795325112829637, 1.000000000000003775 ) ) 
 REPRESENTATION_ITEM ( '' )  );
#21447 = CARTESIAN_POINT ( 'NONE',  ( 1.432654583217639832, 3.458734125000000326, -2.574999998634404541 ) ) ;
#21448 = ORIENTED_EDGE ( 'NONE', *, *, #18165, .F. ) ;
#21449 = DIRECTION ( 'NONE',  ( 0.000000000000000000, 0.000000000000000000, 1.000000000000000000 ) ) ;
#21450 = ORIENTED_EDGE ( 'NONE', *, *, #2620, .T. ) ;
#21451 = PLANE ( 'NONE',  #13352 ) ;
#21452 = VERTEX_POINT ( 'NONE', #5120 ) ;
#21453 = CARTESIAN_POINT ( 'NONE',  ( 58.34606816583844591, 8.825410453826357582, 18.02818770551464667 ) ) ;
#21454 = CARTESIAN_POINT ( 'NONE',  ( -68.75000000218496155, 7.499999999999995559, 16.03553390593273420 ) ) ;
#21455 = CYLINDRICAL_SURFACE ( 'NONE', #17125, 11.00000000000000000 ) ;
#21456 = EDGE_CURVE ( 'NONE', #6956, #17853, #8729, .T. ) ;
#21457 = CARTESIAN_POINT ( 'NONE',  ( 28.39650299071657003, -8.974600000000002353, 10.00000000000008882 ) ) ;
#21458 = CARTESIAN_POINT ( 'NONE',  ( 1.432654583217641386, 3.458734125000000770, 17.37500000136560985 ) ) ;
#21459 = EDGE_CURVE ( 'NONE', #19414, #23443, #5309, .T. ) ;
#21460 = DIRECTION ( 'NONE',  ( -1.000000000000000000, -0.000000000000000000, -0.000000000000000000 ) ) ;
#21461 = CARTESIAN_POINT ( 'NONE',  ( 56.90625000000000711, 12.99999999999999645, 13.75735931288070191 ) ) ;
#21462 = DIRECTION ( 'NONE',  ( -0.000000000000000000, -1.000000000000000000, -0.000000000000000000 ) ) ;
#21463 = CARTESIAN_POINT ( 'NONE',  ( 51.97106816583844591, 6.971812294485350670, 13.82541045382635403 ) ) ;
#21464 = CARTESIAN_POINT ( 'NONE',  ( 2.445694354108820967, -2.445694354108820079, 1.362500001365595903 ) ) ;
#21465 = DIRECTION ( 'NONE',  ( -1.000000000000000000, -7.703719777548943412E-32, 0.000000000000000000 ) ) ;
#21466 = EDGE_CURVE ( 'NONE', #4915, #18669, #3319, .T. ) ;
#21467 = CARTESIAN_POINT ( 'NONE',  ( 70.25000000218493312, 8.964466094067294222, 17.50000000000003908 ) ) ;
#21468 = ORIENTED_EDGE ( 'NONE', *, *, #1603, .T. ) ;
#21469 = CARTESIAN_POINT ( 'NONE',  ( 5.000000000000000888, 0.000000000000000000, 0.000000000000000000 ) ) ;
#21470 = DIRECTION ( 'NONE',  ( -1.000000000000000000, 0.000000000000000000, 0.000000000000000000 ) ) ;
#21471 = VERTEX_POINT ( 'NONE', #6688 ) ;
#21472 = CARTESIAN_POINT ( 'NONE',  ( 2.500000000000000000, 2.357898499370431722, -2.818925648462311528E-15 ) ) ;
#21473 = SURFACE_STYLE_USAGE ( .BOTH. , #16348 ) ;
#21474 = CARTESIAN_POINT ( 'NONE',  ( 1.656854249492380360, 4.000000000000000000, -0.8874999972688129013 ) ) ;
#21475 = CARTESIAN_POINT ( 'NONE',  ( 12.00000000000000000, 0.000000000000000000, -4.000000000000001776 ) ) ;
#21476 = ORIENTED_EDGE ( 'NONE', *, *, #18431, .F. ) ;
#21477 = VERTEX_POINT ( 'NONE', #13894 ) ;
#21478 = SURFACE_SIDE_STYLE ('',( #21598 ) ) ;
#21479 = FACE_OUTER_BOUND ( 'NONE', #13945, .T. ) ;
#21480 = ORIENTED_EDGE ( 'NONE', *, *, #10305, .T. ) ;
#21481 = CARTESIAN_POINT ( 'NONE',  ( 34.67968829071656245, -8.974600000000002353, 5.000000000000079936 ) ) ;
#21482 = CARTESIAN_POINT ( 'NONE',  ( -3.999999999999999112, 0.000000000000000000, 11.00000000000001066 ) ) ;
#21483 = EDGE_CURVE ( 'NONE', #22874, #17270, #21740, .T. ) ;
#21484 = CARTESIAN_POINT ( 'NONE',  ( 65.90000000109246514, 7.933012699999995476, 14.14382582708705094 ) ) ;
#21485 = EDGE_CURVE ( 'NONE', #839, #21889, #21801, .T. ) ;
#21486 = CARTESIAN_POINT ( 'NONE',  ( 71.59999999999999432, 11.76776695296636888, 16.76776695296636532 ) ) ;
#21487 = EDGE_CURVE ( 'NONE', #18107, #3528, #20066, .T. ) ;
#21488 = AXIS2_PLACEMENT_3D ( 'NONE', #4877, #10658, #8376 ) ;
#21489 = CARTESIAN_POINT ( 'NONE',  ( -55.00000000000000000, 15.00000000000000000, 10.00000000000001599 ) ) ;
#21490 = DIRECTION ( 'NONE',  ( 0.000000000000000000, 0.000000000000000000, 1.000000000000000000 ) ) ;
#21491 = CARTESIAN_POINT ( 'NONE',  ( 52.59375000000000711, 11.65685424949236193, 10.99999999999998401 ) ) ;
#21492 = CARTESIAN_POINT ( 'NONE',  ( -2.445694354108819635, -2.445694354108820523, 3.862500001365594571 ) ) ;
#21493 = EDGE_CURVE ( 'NONE', #11604, #10342, #12983, .T. ) ;
#21494 = CARTESIAN_POINT ( 'NONE',  ( 72.50000000000000000, 9.999999999999998224, 14.99999999999999645 ) ) ;
#21495 = CARTESIAN_POINT ( 'NONE',  ( 3.458734125000001214, 1.432654583217640498, 14.00000000136560452 ) ) ;
#21496 = B_SPLINE_CURVE_WITH_KNOTS ( 'NONE', 3,
 ( #10502, #19675, #17781, #9174, #8817, #19919, #23155, #21831, #7127, #12300, #1474, #9050, #3156, #5434, #1595, #1354, #3281, #16115 ),
 .UNSPECIFIED., .F., .F.,
 ( 4, 2, 2, 2, 2, 2, 2, 2, 4 ),
 ( 0.000000000000000000, 0.0006826094070889694504, 0.001365218814177938901, 0.002047828221266908676, 0.002730437628355877801, 0.003413047035444848228, 0.004095656442533819087, 0.004778265849622789080, 0.005460875256711760807 ),
 .UNSPECIFIED. ) ;
#21497 = LINE ( 'NONE', #5108, #4412 ) ;
#21498 = EDGE_CURVE ( 'NONE', #1478, #8676, #4160, .T. ) ;
#21499 = CARTESIAN_POINT ( 'NONE',  ( 54.99999999999992895, -8.499999999999966249, 1.836970198721037478E-15 ) ) ;
#21500 = ORIENTED_EDGE ( 'NONE', *, *, #396, .F. ) ;
#21501 = DIRECTION ( 'NONE',  ( 0.000000000000000000, 0.000000000000000000, -1.000000000000000000 ) ) ;
#21502 = CARTESIAN_POINT ( 'NONE',  ( 2.499999999999999556, -1.975651141462163363, -10.82112760146738673 ) ) ;
#21503 = CARTESIAN_POINT ( 'NONE',  ( 2.499999999999999556, -10.90201369670499965, 1.464956435139506352 ) ) ;
#21504 = EDGE_LOOP ( 'NONE', ( #23561, #17385, #7994, #12785 ) ) ;
#21505 = DIRECTION ( 'NONE',  ( -0.000000000000000000, 0.000000000000000000, -1.000000000000000000 ) ) ;
#21506 = CARTESIAN_POINT ( 'NONE',  ( 71.80000000109247082, 12.06698730000000275, 14.14382582708705094 ) ) ;
#21507 = DIRECTION ( 'NONE',  ( 0.000000000000000000, 0.000000000000000000, 1.000000000000000000 ) ) ;
#21508 = EDGE_LOOP ( 'NONE', ( #6459, #11732, #13335, #8695 ) ) ;
#21509 = CARTESIAN_POINT ( 'NONE',  ( 14.99999999999999645, -10.00000000000000000, -20.00000000000000355 ) ) ;
#21510 = EDGE_LOOP ( 'NONE', ( #17531, #6587, #10812, #3781 ) ) ;
#21511 = CARTESIAN_POINT ( 'NONE',  ( 52.31250000000000711, 14.00000000000000000, 14.99999999999997691 ) ) ;
#21512 = VECTOR ( 'NONE', #17520, 1000.000000000000114 ) ;
#21513 = CARTESIAN_POINT ( 'NONE',  ( 66.65000000218493881, 11.03553390593273598, 12.49999999999999289 ) ) ;
#21514 = CARTESIAN_POINT ( 'NONE',  ( 0.000000000000000000, 1.975651141462390514, -10.82112760146734232 ) ) ;
#21515 = DIRECTION ( 'NONE',  ( 0.000000000000000000, 0.000000000000000000, 1.000000000000000000 ) ) ;
#21516 = EDGE_CURVE ( 'NONE', #16343, #3172, #21749, .T. ) ;
#21517 = CARTESIAN_POINT ( 'NONE',  ( 70.60000000218494165, 9.999999999999998224, 12.49999999999999289 ) ) ;
#21518 = ORIENTED_EDGE ( 'NONE', *, *, #14642, .T. ) ;
#21519 = APPLICATION_CONTEXT ( 'automotive_design' ) ;
#21520 = CARTESIAN_POINT ( 'NONE',  ( 1.520000000000000462, 0.000000000000000000, 0.000000000000000000 ) ) ;
#21521 = CARTESIAN_POINT ( 'NONE',  ( 59.12268183416157541, 12.78030770151606177, 17.87654654797631792 ) ) ;
#21522 = CARTESIAN_POINT ( 'NONE',  ( 4.000000000000000000, 4.898587196589412829E-16, -1.074999997268812679 ) ) ;
#21523 = FACE_OUTER_BOUND ( 'NONE', #15832, .T. ) ;
#21524 = CARTESIAN_POINT ( 'NONE',  ( -2.445694354108818303, -2.445694354108820967, 18.81250000136560629 ) ) ;
#21525 = LINE ( 'NONE', #10446, #4002 ) ;
#21526 = EDGE_CURVE ( 'NONE', #5147, #12674, #22219, .T. ) ;
#21527 = AXIS2_PLACEMENT_3D ( 'NONE', #9235, #21648, #14625 ) ;
#21528 = CARTESIAN_POINT ( 'NONE',  ( 24.42673246966726452, -11.25000000000000355, 5.000000000000079936 ) ) ;
#21529 = ORIENTED_EDGE ( 'NONE', *, *, #14204, .T. ) ;
#21530 = CARTESIAN_POINT ( 'NONE',  ( -3.298587526675563097, 1.112609898547286980, -3.295601554149322876 ) ) ;
#21531 = CARTESIAN_POINT ( 'NONE',  ( 55.12500000000000711, 12.12132034355964727, 17.12132034355963484 ) ) ;
#21532 = CARTESIAN_POINT ( 'NONE',  ( -1.656854249492379472, 4.000000000000000000, 10.93750000273119660 ) ) ;
#21533 =( LENGTH_UNIT ( ) NAMED_UNIT ( * ) SI_UNIT ( .MILLI., .METRE. ) );
#21534 = VERTEX_POINT ( 'NONE', #7170 ) ;
#21535 = PLANE ( 'NONE',  #14761 ) ;
#21536 = CARTESIAN_POINT ( 'NONE',  ( -3.458734125000000326, 1.432654583217640276, -2.324999998634404097 ) ) ;
#21537 = CARTESIAN_POINT ( 'NONE',  ( 2.000000000000005329, -3.464101615137751722, 0.000000000000000000 ) ) ;
#21538 = EDGE_LOOP ( 'NONE', ( #15965, #12312, #3473, #20119, #9647 ) ) ;
#21539 = CARTESIAN_POINT ( 'NONE',  ( -4.000000000000000000, 2.309401076758498483, -3.433295621305379353 ) ) ;
#21540 = ORIENTED_EDGE ( 'NONE', *, *, #12057, .F. ) ;
#21541 = DIRECTION ( 'NONE',  ( -7.087422195345011518E-32, -1.000000000000000000, 0.000000000000000000 ) ) ;
#21542 = ORIENTED_EDGE ( 'NONE', *, *, #22427, .T. ) ;
#21543 = CARTESIAN_POINT ( 'NONE',  ( -3.999999999999999112, 0.000000000000000000, 20.00000000000001066 ) ) ;
#21544 = CARTESIAN_POINT ( 'NONE',  ( -2.000000000000001776, 0.000000000000000000, 0.000000000000000000 ) ) ;
#21545 = DIRECTION ( 'NONE',  ( -0.8660254037844382635, 0.5000000000000006661, 0.000000000000000000 ) ) ;
#21546 =( NAMED_UNIT ( * ) PLANE_ANGLE_UNIT ( ) SI_UNIT ( $, .RADIAN. ) );
#21547 = CARTESIAN_POINT ( 'NONE',  ( -0.6920835326022555245, -4.454600218803899558, -3.597382984111586079 ) ) ;
#21548 = CARTESIAN_POINT ( 'NONE',  ( -71.70000000000000284, 9.999999999999998224, 17.49999999999999645 ) ) ;
#21549 = CARTESIAN_POINT ( 'NONE',  ( -4.000000000000000000, -2.309401076758515803, -0.4999999999999995559 ) ) ;
#21550 = EDGE_CURVE ( 'NONE', #12867, #11644, #16615, .T. ) ;
#21551 = CARTESIAN_POINT ( 'NONE',  ( 60.00000000000000711, 11.02697561308437812, 18.23285838809245618 ) ) ;
#21552 = CARTESIAN_POINT ( 'NONE',  ( 2.445694354108820967, -2.445694354108820079, 0.3625000013655968467 ) ) ;
#21553 = CARTESIAN_POINT ( 'NONE',  ( -67.75000000218496155, 11.03553390593276617, 17.49999999999997513 ) ) ;
#21554 = CARTESIAN_POINT ( 'NONE',  ( 4.999999999999999112, -7.958834565716820464, 7.593217523260553214 ) ) ;
#21555 = CARTESIAN_POINT ( 'NONE',  ( 1.872352939448454495E-15, -3.458734125000000326, 17.68750000136560274 ) ) ;
#21556 = CARTESIAN_POINT ( 'NONE',  ( 18.14354716966726144, -11.25000000000000355, 10.00000000000008882 ) ) ;
#21557 = ORIENTED_EDGE ( 'NONE', *, *, #12783, .F. ) ;
#21558 = CARTESIAN_POINT ( 'NONE',  ( -70.70000000109247651, 7.933012699999995476, 14.14382582708705094 ) ) ;
#21559 = EDGE_LOOP ( 'NONE', ( #22899, #5807 ) ) ;
#21560 = CARTESIAN_POINT ( 'NONE',  ( 57.99768183416157541, 12.87654654797631792, 12.21969229848393113 ) ) ;
#21561 = CARTESIAN_POINT ( 'NONE',  ( -68.60000000109248219, 12.06698730000000275, 14.14382582708705094 ) ) ;
#21562 = CARTESIAN_POINT ( 'NONE',  ( 1.236993788156008760E-15, 0.000000000000000000, 13.70000000000000817 ) ) ;
#21563 = CARTESIAN_POINT ( 'NONE',  ( 2.445694354108820079, 2.445694354108820523, -1.637499998634403209 ) ) ;
#21564 = ORIENTED_EDGE ( 'NONE', *, *, #1168, .F. ) ;
#21565 = CYLINDRICAL_SURFACE ( 'NONE', #14857, 4.000000000000000000 ) ;
#21566 = ORIENTED_EDGE ( 'NONE', *, *, #7060, .T. ) ;
#21567 = CARTESIAN_POINT ( 'NONE',  ( 71.20000000000000284, 8.232233047033629347, 13.23223304703362402 ) ) ;
#21568 = ORIENTED_EDGE ( 'NONE', *, *, #8240, .T. ) ;
#21569 = CARTESIAN_POINT ( 'NONE',  ( 51.68981816583844591, 9.931948859054354983, 11.99999999999999645 ) ) ;
#21570 = VECTOR ( 'NONE', #7131, 1000.000000000000000 ) ;
#21571 = CARTESIAN_POINT ( 'NONE',  ( -67.15000000218495302, 7.499999999999995559, 16.03553390593273420 ) ) ;
#21572 = VECTOR ( 'NONE', #22507, 1000.000000000000000 ) ;
#21573 = DIRECTION ( 'NONE',  ( 0.000000000000000000, 0.000000000000000000, -1.000000000000000000 ) ) ;
#21574 = CARTESIAN_POINT ( 'NONE',  ( 55.00000000000000711, -15.00000000000000000, 10.00000000000000000 ) ) ;
#21575 = CARTESIAN_POINT ( 'NONE',  ( 3.458734125000002546, -1.432654583217639610, 16.12500000136560629 ) ) ;
#21576 = FACE_OUTER_BOUND ( 'NONE', #21842, .T. ) ;
#21577 = CYLINDRICAL_SURFACE ( 'NONE', #502, 4.000000000000000000 ) ;
#21578 = CARTESIAN_POINT ( 'NONE',  ( 4.000000000000000000, 0.000000000000000000, 19.04999999999996874 ) ) ;
#21579 = CARTESIAN_POINT ( 'NONE',  ( 56.43750000000000000, 10.00000000000000711, 17.99999999999999645 ) ) ;
#21580 = CARTESIAN_POINT ( 'NONE',  ( -3.458734125000000326, -1.432654583217642497, -2.949999998634404985 ) ) ;
#21581 = CARTESIAN_POINT ( 'NONE',  ( -2.828427124746189403, 2.828427124746190291, 19.00000000273119838 ) ) ;
#21582 = CARTESIAN_POINT ( 'NONE',  ( -68.29999999999999716, 12.50000000000000000, 14.99999999999999645 ) ) ;
#21583 = VECTOR ( 'NONE', #9433, 999.9999999999997726 ) ;
#21584 = ORIENTED_EDGE ( 'NONE', *, *, #4567, .T. ) ;
#21585 = CARTESIAN_POINT ( 'NONE',  ( -4.000000000000000000, -0.7890432684750890990, -0.04868663549882315533 ) ) ;
#21586 = DIRECTION ( 'NONE',  ( 0.000000000000000000, -6.938893903907226800E-15, 1.000000000000000000 ) ) ;
#21587 = VERTEX_POINT ( 'NONE', #7411 ) ;
#21588 = CARTESIAN_POINT ( 'NONE',  ( 57.75000000000000000, 7.878679656440361612, 17.12132034355964549 ) ) ;
#21589 = VECTOR ( 'NONE', #10511, 1000.000000000000000 ) ;
#21590 = PRODUCT_CONTEXT ( 'NONE', #21378, 'mechanical' ) ;
#21591 = CARTESIAN_POINT ( 'NONE',  ( 4.000000000000000888, -1.656854249492379694, 1.862500002731187765 ) ) ;
#21592 = TOROIDAL_SURFACE ( 'NONE', #5161, 2.700000000000000622, 0.2000000000000000111 ) ;
#21593 = DIRECTION ( 'NONE',  ( 0.000000000000000000, 0.000000000000000000, -1.000000000000000000 ) ) ;
#21594 = ORIENTED_EDGE ( 'NONE', *, *, #18358, .F. ) ;
#21595 = CARTESIAN_POINT ( 'NONE',  ( 1.656854249492384135, -3.999999999999999112, 15.31250000000000888 ) ) ;
#21596 = EDGE_LOOP ( 'NONE', ( #5649, #6237, #20607, #23466 ) ) ;
#21597 = EDGE_CURVE ( 'NONE', #17601, #21119, #1465, .T. ) ;
#21598 = SURFACE_STYLE_FILL_AREA ( #12549 ) ;
#21599 = CARTESIAN_POINT ( 'NONE',  ( -66.69999999999998863, 12.50000000000000000, 14.99999999999999645 ) ) ;
#21600 = ORIENTED_EDGE ( 'NONE', *, *, #22120, .T. ) ;
#21601 = CARTESIAN_POINT ( 'NONE',  ( -55.00000000000000000, 15.00000000000000000, 10.00000000000001599 ) ) ;
#21602 = CARTESIAN_POINT ( 'NONE',  ( 8.718769219667262149, -11.25000000000000355, 5.000000000000079936 ) ) ;
#21603 = VERTEX_POINT ( 'NONE', #10785 ) ;
#21604 = EDGE_CURVE ( 'NONE', #15248, #15525, #18059, .T. ) ;
#21605 = CARTESIAN_POINT ( 'NONE',  ( 2.499999999999999556, 7.593217523260583413, 7.958834565716794707 ) ) ;
#21606 = VECTOR ( 'NONE', #10097, 1000.000000000000000 ) ;
#21607 = CARTESIAN_POINT ( 'NONE',  ( 71.24999999999998579, 8.964466094067258695, 12.49999999999999289 ) ) ;
#21608 = AXIS2_PLACEMENT_3D ( 'NONE', #2943, #4517, #1032 ) ;
#21609 = DIRECTION ( 'NONE',  ( -0.000000000000000000, -0.000000000000000000, -1.000000000000000000 ) ) ;
#21610 = CARTESIAN_POINT ( 'NONE',  ( 69.80000000218494449, 9.999999999999998224, 12.49999999999999289 ) ) ;
#21611 = CARTESIAN_POINT ( 'NONE',  ( 57.97106816583845301, 5.971812294485345340, 13.41119689145326710 ) ) ;
#21612 = CARTESIAN_POINT ( 'NONE',  ( -3.458734125000000326, 0.000000000000000000, 3.737500001365594571 ) ) ;
#21613 = FILL_AREA_STYLE_COLOUR ( '', #9552 ) ;
#21614 = CARTESIAN_POINT ( 'NONE',  ( -3.458734124999998105, 1.432654583217640276, 14.37500000136560452 ) ) ;
#21615 = DIRECTION ( 'NONE',  ( 0.000000000000000000, 0.5000000000000009992, 0.8660254037844380415 ) ) ;
#21616 = AXIS2_PLACEMENT_3D ( 'NONE', #17116, #15219, #15458 ) ;
#21617 = VECTOR ( 'NONE', #6572, 1000.000000000000000 ) ;
#21618 = CARTESIAN_POINT ( 'NONE',  ( -70.40000000218495302, 7.499999999999996447, 14.99999999999999645 ) ) ;
#21619 = ORIENTED_EDGE ( 'NONE', *, *, #2470, .T. ) ;
#21620 = FACE_OUTER_BOUND ( 'NONE', #1983, .T. ) ;
#21621 = CARTESIAN_POINT ( 'NONE',  ( -6.500000000000002665, 1.277696550142690235, -3.643982548855206449 ) ) ;
#21622 = FACE_OUTER_BOUND ( 'NONE', #11750, .T. ) ;
#21623 = ORIENTED_EDGE ( 'NONE', *, *, #21636, .T. ) ;
#21624 = EDGE_CURVE ( 'NONE', #4004, #7647, #10893, .T. ) ;
#21625 = CYLINDRICAL_SURFACE ( 'NONE', #17513, 4.000000000000001776 ) ;
#21626 = CIRCLE ( 'NONE', #7124, 2.500000000000007550 ) ;
#21627 = EDGE_CURVE ( 'NONE', #10924, #15256, #6467, .T. ) ;
#21628 = ORIENTED_EDGE ( 'NONE', *, *, #119, .F. ) ;
#21629 = CARTESIAN_POINT ( 'NONE',  ( 44.00000000000000711, -9.261618637464055226, 10.00000000000008882 ) ) ;
#21630 = VERTEX_POINT ( 'NONE', #7648 ) ;
#21631 = FACE_OUTER_BOUND ( 'NONE', #15428, .T. ) ;
#21632 = EDGE_LOOP ( 'NONE', ( #20297, #5269 ) ) ;
#21633 = CARTESIAN_POINT ( 'NONE',  ( 55.31250000000000711, 14.00000000000000000, 14.99999999999997691 ) ) ;
#21634 = EDGE_CURVE ( 'NONE', #16343, #9962, #12809, .T. ) ;
#21635 = CARTESIAN_POINT ( 'NONE',  ( 69.35000000218495586, 11.03553390593273598, 17.50000000000000355 ) ) ;
#21636 = EDGE_CURVE ( 'NONE', #7520, #19202, #18515, .T. ) ;
#21637 = CARTESIAN_POINT ( 'NONE',  ( 4.999999999999999112, -8.264486777890139635, 4.472189673936757259 ) ) ;
#21638 = PLANE ( 'NONE',  #12568 ) ;
#21639 = DIRECTION ( 'NONE',  ( 1.000000000000000000, 0.000000000000000000, -0.000000000000000000 ) ) ;
#21640 = EDGE_LOOP ( 'NONE', ( #21352, #21239, #8861, #20807 ) ) ;
#21641 = LINE ( 'NONE', #5372, #1871 ) ;
#21642 = CARTESIAN_POINT ( 'NONE',  ( 53.21643183416158251, 12.97181229448535689, 16.31069182806490758 ) ) ;
#21643 = CARTESIAN_POINT ( 'NONE',  ( -1.600000000000004086, 0.000000000000000000, -8.073750000000021743 ) ) ;
#21644 = CARTESIAN_POINT ( 'NONE',  ( 66.70000000109246230, 9.143825827087049163, 17.06698729999999742 ) ) ;
#21645 = CARTESIAN_POINT ( 'NONE',  ( -1.647987302177966740E-14, -7.505553499465137612, -0.5805565836007695601 ) ) ;
#21646 = CARTESIAN_POINT ( 'NONE',  ( 0.2500000000000002220, 0.000000000000000000, 0.000000000000000000 ) ) ;
#21647 = ORIENTED_EDGE ( 'NONE', *, *, #10605, .T. ) ;
#21648 = DIRECTION ( 'NONE',  ( -0.000000000000000000, -0.000000000000000000, 1.000000000000000000 ) ) ;
#21649 = CARTESIAN_POINT ( 'NONE',  ( 55.87500000000000711, 7.878679656440349177, 12.87867965644035984 ) ) ;
#21650 = EDGE_CURVE ( 'NONE', #7387, #15758, #8406, .T. ) ;
#21651 = CARTESIAN_POINT ( 'NONE',  ( 66.69999999999998863, 12.50000000000000000, 14.99999999999999645 ) ) ;
#21652 =( NAMED_UNIT ( * ) SI_UNIT ( $, .STERADIAN. ) SOLID_ANGLE_UNIT ( ) );
#21653 = ORIENTED_EDGE ( 'NONE', *, *, #9683, .T. ) ;
#21654 = DIRECTION ( 'NONE',  ( 0.000000000000000000, 0.000000000000000000, -1.000000000000000000 ) ) ;
#21655 = CARTESIAN_POINT ( 'NONE',  ( 2.445694354108820523, -2.445694354108820079, -2.887499998634404097 ) ) ;
#21656 = CARTESIAN_POINT ( 'NONE',  ( -65.00000000000000000, 9.999999999999998224, 12.49999999999999289 ) ) ;
#21657 = SHAPE_REPRESENTATION ( 'radial cylindrical roller bearing_iso_ISO 15 RCR - 1712 - 24,SI,NC,24', ( #7318 ), #21725 ) ;
#21658 = ADVANCED_FACE ( 'NONE', ( #9217 ), #4543, .T. ) ;
#21659 = ORIENTED_EDGE ( 'NONE', *, *, #3176, .F. ) ;
#21660 = DIRECTION ( 'NONE',  ( -1.000000000000000000, 0.000000000000000000, -0.000000000000000000 ) ) ;
#21661 = EDGE_LOOP ( 'NONE', ( #5893, #11241, #15442 ) ) ;
#21662 = CARTESIAN_POINT ( 'NONE',  ( 9.920644283265380691E-16, 4.000000000000000000, 18.75000000000001066 ) ) ;
#21663 = CARTESIAN_POINT ( 'NONE',  ( 2.828427124746192067, -2.828427124746189847, 17.37500000000001066 ) ) ;
#21664 = EDGE_CURVE ( 'NONE', #22158, #4844, #77, .T. ) ;
#21665 = FACE_OUTER_BOUND ( 'NONE', #8028, .T. ) ;
#21666 = EDGE_CURVE ( 'NONE', #7447, #129, #23482, .T. ) ;
#21667 = CARTESIAN_POINT ( 'NONE',  ( 27.50000000000000000, 1.500000000000003109, -31.01025403784446510 ) ) ;
#21668 = CARTESIAN_POINT ( 'NONE',  ( 0.000000000000000000, 0.000000000000000000, 19.04999999999996874 ) ) ;
#21669 = PLANE ( 'NONE',  #11777 ) ;
#21670 = CARTESIAN_POINT ( 'NONE',  ( -67.54999999999999716, 12.50000000000000000, 16.03553390593273420 ) ) ;
#21671 = FACE_OUTER_BOUND ( 'NONE', #11355, .T. ) ;
#21672 = CARTESIAN_POINT ( 'NONE',  ( 60.00000000000000000, 13.97680642442999854, 14.92529509588244352 ) ) ;
#21673 = CARTESIAN_POINT ( 'NONE',  ( 4.207491450040567571, -2.029819825146485179, -3.671670828759567407 ) ) ;
#21674 = AXIS2_PLACEMENT_3D ( 'NONE', #9017, #6, #12620 ) ;
#21675 = CARTESIAN_POINT ( 'NONE',  ( -2.445694354108820523, 2.445694354108820523, -3.137499998634402765 ) ) ;
#21676 = CARTESIAN_POINT ( 'NONE',  ( -66.30000000109247082, 10.85617417291294551, 12.93301269999999192 ) ) ;
#21677 = CARTESIAN_POINT ( 'NONE',  ( 67.79999999999999716, 8.232233047033627571, 16.76776695296636532 ) ) ;
#21678 = CARTESIAN_POINT ( 'NONE',  ( -3.458734124999998993, -1.432654583217642497, 16.50000000136560629 ) ) ;
#21679 = DIRECTION ( 'NONE',  ( -1.000000000000000000, -7.703719777548943412E-32, 0.000000000000000000 ) ) ;
#21680 = EDGE_LOOP ( 'NONE', ( #12552, #21392, #4766, #14049 ) ) ;
#21681 = CIRCLE ( 'NONE', #10253, 4.714285714285714413 ) ;
#21682 = CARTESIAN_POINT ( 'NONE',  ( -72.00000000109248788, 10.85617417291294551, 17.06698730000000097 ) ) ;
#21683 = ORIENTED_EDGE ( 'NONE', *, *, #15078, .F. ) ;
#21684 = CARTESIAN_POINT ( 'NONE',  ( 53.40393183416157541, 14.02818770551463956, 13.41119689145323335 ) ) ;
#21685 = CARTESIAN_POINT ( 'NONE',  ( -68.00000000109247367, 10.85617417291294551, 17.06698729999999742 ) ) ;
#21686 = CARTESIAN_POINT ( 'NONE',  ( 2.500000000000000444, 0.000000000000000000, -25.03750572909317285 ) ) ;
#21687 = EDGE_LOOP ( 'NONE', ( #10217, #11213, #21743, #9812, #8143 ) ) ;
#21688 = MECHANICAL_DESIGN_GEOMETRIC_PRESENTATION_REPRESENTATION (  '', ( #18641 ), #4504 ) ;
#21689 = AXIS2_PLACEMENT_3D ( 'NONE', #5301, #3260, #19781 ) ;
#21690 = FACE_OUTER_BOUND ( 'NONE', #3166, .T. ) ;
#21691 = ORIENTED_EDGE ( 'NONE', *, *, #18137, .F. ) ;
#21692 = FACE_OUTER_BOUND ( 'NONE', #16069, .T. ) ;
#21693 = ORIENTED_EDGE ( 'NONE', *, *, #4335, .T. ) ;
#21694 = ADVANCED_FACE ( 'NONE', ( #9682 ), #5583, .F. ) ;
#21695 = CARTESIAN_POINT ( 'NONE',  ( 59.06250000000000711, 6.999999999999997335, 15.00000000000000533 ) ) ;
#21696 = ADVANCED_FACE ( 'NONE', ( #6069 ), #2706, .F. ) ;
#21697 = CARTESIAN_POINT ( 'NONE',  ( -71.50000000109248788, 7.933012699999995476, 14.14382582708705094 ) ) ;
#21698 = CARTESIAN_POINT ( 'NONE',  ( -69.80000000109247082, 10.85617417291294551, 17.06698729999999742 ) ) ;
#21699 = CARTESIAN_POINT ( 'NONE',  ( 3.458734125000002546, -1.432654583217639610, 17.12500000136560629 ) ) ;
#21700 = CARTESIAN_POINT ( 'NONE',  ( -2.828427124746188515, -2.828427124746190735, 10.25000000273119660 ) ) ;
#21701 = CARTESIAN_POINT ( 'NONE',  ( 52.03124999999999289, 11.24264068711929276, 18.00000000000000355 ) ) ;
#21702 = CARTESIAN_POINT ( 'NONE',  ( 27.50000000000000000, 1.500000000000003109, -33.66025403784446723 ) ) ;
#21703 = AXIS2_PLACEMENT_3D ( 'NONE', #3057, #12311, #19574 ) ;
#21704 = VECTOR ( 'NONE', #13132, 1000.000000000000000 ) ;
#21705 = CARTESIAN_POINT ( 'NONE',  ( 58.96875000000000711, 6.999999999999992895, 13.75735931288071967 ) ) ;
#21706 = CARTESIAN_POINT ( 'NONE',  ( 1.432654583217642275, -3.458734124999999882, -1.699999998634404097 ) ) ;
#21707 = CARTESIAN_POINT ( 'NONE',  ( 1.656854249492381470, 4.000000000000000000, 18.81250000273119838 ) ) ;
#21708 = ORIENTED_EDGE ( 'NONE', *, *, #524, .F. ) ;
#21709 = CARTESIAN_POINT ( 'NONE',  ( 0.7277801532338118440, -9.000000000000003553, 5.000000000000079936 ) ) ;
#21710 = DIRECTION ( 'NONE',  ( 0.000000000000000000, 0.000000000000000000, -1.000000000000000000 ) ) ;
#21711 = EDGE_LOOP ( 'NONE', ( #15933, #12077, #8794, #6425, #15970 ) ) ;
#21712 = CARTESIAN_POINT ( 'NONE',  ( 52.78125000000000711, 8.757359312880703683, 11.99999999999999822 ) ) ;
#21713 = CARTESIAN_POINT ( 'NONE',  ( 4.000000000000000888, -1.656854249492379694, 0.8625000027311868767 ) ) ;
#21714 = DIRECTION ( 'NONE',  ( -1.000000000000000000, -0.000000000000000000, -0.000000000000000000 ) ) ;
#21715 = ORIENTED_EDGE ( 'NONE', *, *, #22539, .T. ) ;
#21716 = CARTESIAN_POINT ( 'NONE',  ( -2.828427124746189403, 2.828427124746190291, 16.87500000000001066 ) ) ;
#21717 = ORIENTED_EDGE ( 'NONE', *, *, #14061, .T. ) ;
#21718 = VECTOR ( 'NONE', #8297, 1000.000000000000000 ) ;
#21719 = CARTESIAN_POINT ( 'NONE',  ( -4.000000000000000888, 1.656854249492380582, -2.637499997268812013 ) ) ;
#21720 = VERTEX_POINT ( 'NONE', #11364 ) ;
#21721 = DIRECTION ( 'NONE',  ( -1.000000000000000000, -7.703719777548943412E-32, 0.000000000000000000 ) ) ;
#21722 = AXIS2_PLACEMENT_3D ( 'NONE', #19426, #1105, #13718 ) ;
#21723 = VECTOR ( 'NONE', #11357, 1000.000000000000000 ) ;
#21724 = FACE_OUTER_BOUND ( 'NONE', #13365, .T. ) ;
#21725 =( GEOMETRIC_REPRESENTATION_CONTEXT ( 3 ) GLOBAL_UNCERTAINTY_ASSIGNED_CONTEXT ( ( #14099 ) ) GLOBAL_UNIT_ASSIGNED_CONTEXT ( ( #7258, #14215, #14574 ) ) REPRESENTATION_CONTEXT ( 'NONE', 'WORKASPACE' ) );
#21726 = VERTEX_POINT ( 'NONE', #11842 ) ;
#21727 = CARTESIAN_POINT ( 'NONE',  ( 66.20000000109247651, 12.06698730000000275, 14.14382582708705094 ) ) ;
#21728 = CARTESIAN_POINT ( 'NONE',  ( 70.54999999999999716, 11.03553390593273598, 12.49999999999999289 ) ) ;
#21729 = CARTESIAN_POINT ( 'NONE',  ( -3.250000000000004441, 5.629165124598849879, -3.700000000000000178 ) ) ;
#21730 = CIRCLE ( 'NONE', #19822, 8.073750000000021743 ) ;
#21731 = EDGE_CURVE ( 'NONE', #10312, #4233, #13157, .T. ) ;
#21732 = CARTESIAN_POINT ( 'NONE',  ( 56.56481816583843170, 5.999999999999996447, 15.06805114094564502 ) ) ;
#21733 = CARTESIAN_POINT ( 'NONE',  ( 1.432654583217639832, 3.458734125000000326, 1.425000001365596791 ) ) ;
#21734 = DIRECTION ( 'NONE',  ( -1.000000000000000000, -0.000000000000000000, -0.000000000000000000 ) ) ;
#21735 = CARTESIAN_POINT ( 'NONE',  ( -3.458734124999998105, -1.432654583217642275, 10.50000000136560452 ) ) ;
#21736 = LINE ( 'NONE', #5348, #9020 ) ;
#21737 = PLANE ( 'NONE',  #6729 ) ;
#21738 = ORIENTED_EDGE ( 'NONE', *, *, #17970, .F. ) ;
#21739 = DIRECTION ( 'NONE',  ( -1.000000000000000000, -4.625929269271486900E-16, 0.000000000000000000 ) ) ;
#21740 = CIRCLE ( 'NONE', #17168, 8.749000000000002331 ) ;
#21741 = CARTESIAN_POINT ( 'NONE',  ( 2.100000000000000089, 0.000000000000000000, -0.2800830152838844622 ) ) ;
#21742 = CARTESIAN_POINT ( 'NONE',  ( -20.00005080000000035, 5.400000000000000355, 0.000000000000000000 ) ) ;
#21743 = ORIENTED_EDGE ( 'NONE', *, *, #23195, .F. ) ;
#21744 = ORIENTED_EDGE ( 'NONE', *, *, #4343, .F. ) ;
#21745 = DIRECTION ( 'NONE',  ( 0.000000000000000000, 0.000000000000000000, 1.000000000000000000 ) ) ;
#21746 = VECTOR ( 'NONE', #17834, 1000.000000000000000 ) ;
#21747 = CARTESIAN_POINT ( 'NONE',  ( 56.81250000000000000, 14.00000000000000000, 14.99999999999997691 ) ) ;
#21748 = EDGE_LOOP ( 'NONE', ( #6634, #1647, #3665, #13074 ) ) ;
#21749 = LINE ( 'NONE', #3669, #9541 ) ;
#21750 = VERTEX_POINT ( 'NONE', #7874 ) ;
#21751 = CIRCLE ( 'NONE', #22140, 6.760799999999997034 ) ;
#21752 = CARTESIAN_POINT ( 'NONE',  ( 53.25000000000000711, 7.171572875253819923, 17.82842712474619873 ) ) ;
#21753 = CARTESIAN_POINT ( 'NONE',  ( 66.85000000218495586, 12.50000000000000000, 16.03553390593273420 ) ) ;
#21754 = AXIS2_PLACEMENT_3D ( 'NONE', #14548, #19899, #10720 ) ;
#21755 =( GEOMETRIC_REPRESENTATION_CONTEXT ( 3 ) GLOBAL_UNCERTAINTY_ASSIGNED_CONTEXT ( ( #21245 ) ) GLOBAL_UNIT_ASSIGNED_CONTEXT ( ( #21286, #21415, #21652 ) ) REPRESENTATION_CONTEXT ( 'NONE', 'WORKASPACE' ) );
#21756 = LINE ( 'NONE', #18178, #2662 ) ;
#21757 = CARTESIAN_POINT ( 'NONE',  ( -68.54999999999998295, 8.964466094067287116, 17.50000000000002487 ) ) ;
#21758 = DIRECTION ( 'NONE',  ( 0.000000000000000000, 1.224646799147353207E-16, 1.000000000000000000 ) ) ;
#21759 = ORIENTED_EDGE ( 'NONE', *, *, #14442, .F. ) ;
#21760 = CARTESIAN_POINT ( 'NONE',  ( 4.000000000000000888, 1.656854249492381248, 18.68750000273119483 ) ) ;
#21761 = EDGE_CURVE ( 'NONE', #12101, #20275, #15081, .T. ) ;
#21762 = DIRECTION ( 'NONE',  ( 7.087422195345011518E-32, 1.000000000000000000, 0.000000000000000000 ) ) ;
#21763 = EDGE_CURVE ( 'NONE', #18607, #17296, #22457, .T. ) ;
#21764 = CARTESIAN_POINT ( 'NONE',  ( 57.06018183416157541, 5.999999999999996447, 14.93194885905437808 ) ) ;
#21765 = CARTESIAN_POINT ( 'NONE',  ( 3.820581514278380109, 0.3741733693073286959, 2.039999999999999591 ) ) ;
#21766 = AXIS2_PLACEMENT_3D ( 'NONE', #21637, #19961, #5241 ) ;
#21767 = CARTESIAN_POINT ( 'NONE',  ( 67.35000000109246798, 11.46158073645647235, 16.46158073645647235 ) ) ;
#21768 = CARTESIAN_POINT ( 'NONE',  ( -67.84999999999999432, 7.499999999999996447, 16.03553390593273775 ) ) ;
#21769 = VECTOR ( 'NONE', #16485, 1000.000000000000000 ) ;
#21770 = DIRECTION ( 'NONE',  ( 1.000000000000000000, 7.703719777548943412E-32, 0.000000000000000000 ) ) ;
#21771 = ORIENTED_EDGE ( 'NONE', *, *, #22860, .F. ) ;
#21772 = CARTESIAN_POINT ( 'NONE',  ( -2.117863837641483646E-16, 3.458734125000000770, -3.295601554149324208 ) ) ;
#21773 = CARTESIAN_POINT ( 'NONE',  ( 54.18750000000000711, 9.999999999999989342, 11.99999999999999467 ) ) ;
#21774 = DIRECTION ( 'NONE',  ( 0.000000000000000000, 0.8090169943749445647, 0.5877852522924772449 ) ) ;
#21775 = CARTESIAN_POINT ( 'NONE',  ( -72.39999999999999147, 11.76776695296636888, 16.76776695296636532 ) ) ;
#21776 = EDGE_CURVE ( 'NONE', #19904, #9536, #2351, .T. ) ;
#21777 = ORIENTED_EDGE ( 'NONE', *, *, #7093, .F. ) ;
#21778 = DIRECTION ( 'NONE',  ( 0.3420201433256622181, 0.9396926207859107594, -6.162975822039141593E-32 ) ) ;
#21779 = PLANE ( 'NONE',  #9918 ) ;
#21780 = CARTESIAN_POINT ( 'NONE',  ( 4.000000000000000000, -2.309401076758516691, -0.4999999999999995559 ) ) ;
#21781 = COLOUR_RGB ( '', 0.40784314, 0.44705882, 0.49803922) ;
#21782 = ORIENTED_EDGE ( 'NONE', *, *, #9360, .T. ) ;
#21783 = CARTESIAN_POINT ( 'NONE',  ( 2.499999999999999556, 4.762163868918273479, 9.915734732513236338 ) ) ;
#21784 = VERTEX_POINT ( 'NONE', #6315 ) ;
#21785 = VERTEX_POINT ( 'NONE', #13276 ) ;
#21786 = CARTESIAN_POINT ( 'NONE',  ( 1.656854249492381470, 4.000000000000000000, 18.68750000000001066 ) ) ;
#21787 = CARTESIAN_POINT ( 'NONE',  ( -1.656854249492380138, -3.999999999999999112, 18.18750000000001066 ) ) ;
#21788 = CARTESIAN_POINT ( 'NONE',  ( -66.34999999999999432, 7.499999999999996447, 13.96446609406725514 ) ) ;
#21789 = CIRCLE ( 'NONE', #16459, 4.000000000000001776 ) ;
#21790 = VECTOR ( 'NONE', #23040, 1000.000000000000000 ) ;
#21791 = FACE_OUTER_BOUND ( 'NONE', #10131, .T. ) ;
#21792 = EDGE_CURVE ( 'NONE', #23080, #1931, #18639, .T. ) ;
#21793 =( NAMED_UNIT ( * ) SI_UNIT ( $, .STERADIAN. ) SOLID_ANGLE_UNIT ( ) );
#21794 = FACE_OUTER_BOUND ( 'NONE', #106, .T. ) ;
#21795 = AXIS2_PLACEMENT_3D ( 'NONE', #20054, #3659, #5582 ) ;
#21796 = CARTESIAN_POINT ( 'NONE',  ( -67.45000000000000284, 12.50000000000000000, 13.96446609406725869 ) ) ;
#21797 = EDGE_CURVE ( 'NONE', #23527, #19804, #4183, .T. ) ;
#21798 = DIRECTION ( 'NONE',  ( -1.000000000000000000, -7.703719777548943412E-32, 0.000000000000000000 ) ) ;
#21799 = CARTESIAN_POINT ( 'NONE',  ( 3.458734125000002102, -1.432654583217639610, 17.87500000136560274 ) ) ;
#21800 = CARTESIAN_POINT ( 'NONE',  ( 4.999999999999999112, 0.000000000000000000, 0.000000000000000000 ) ) ;
#21801 =( BOUNDED_CURVE ( )  B_SPLINE_CURVE ( 2, ( #5712, #9091, #18172, #14966, #21868, #5473, #194, #14839, #23564 ),
 .UNSPECIFIED., .F., .F. ) 
 B_SPLINE_CURVE_WITH_KNOTS ( ( 3, 2, 2, 2, 3 ),
 ( 0.1499999999999999944, 0.1625000000000000056, 0.1749999999999999889, 0.1875000000000000000, 0.2000000000000000111 ),
 .UNSPECIFIED. ) 
 CURVE ( )  GEOMETRIC_REPRESENTATION_ITEM ( )  RATIONAL_B_SPLINE_CURVE ( ( 1.000000000000000000, 0.9238795325112867385, 1.000000000000000000, 0.9238795325112867385, 1.000000000000000000, 0.9238795325112867385, 1.000000000000000000, 0.9238795325112867385, 1.000000000000000000 ) ) 
 REPRESENTATION_ITEM ( '' )  );
#21802 = CARTESIAN_POINT ( 'NONE',  ( -3.458734125000000326, -1.432654583217642497, -2.949999998634404985 ) ) ;
#21803 = CARTESIAN_POINT ( 'NONE',  ( -66.80000000109247082, 7.933012699999995476, 15.85617417291294196 ) ) ;
#21804 = DIRECTION ( 'NONE',  ( 0.000000000000000000, -6.938893903907225222E-15, 1.000000000000000000 ) ) ;
#21805 = CARTESIAN_POINT ( 'NONE',  ( 3.458734125000001214, 1.432654583217640498, 16.00000000136560629 ) ) ;
#21806 = CARTESIAN_POINT ( 'NONE',  ( 2.500000000000000000, 0.000000000000000000, 0.000000000000000000 ) ) ;
#21807 = ADVANCED_FACE ( 'NONE', ( #15195 ), #20668, .T. ) ;
#21808 = EDGE_CURVE ( 'NONE', #10807, #22879, #9931, .T. ) ;
#21809 = ORIENTED_EDGE ( 'NONE', *, *, #48, .T. ) ;
#21810 = CARTESIAN_POINT ( 'NONE',  ( -68.30000000109247082, 7.933012699999995476, 14.14382582708705094 ) ) ;
#21811 = ORIENTED_EDGE ( 'NONE', *, *, #5699, .F. ) ;
#21812 = CARTESIAN_POINT ( 'NONE',  ( 53.68518183416157541, 10.06805114094561659, 10.99999999999999645 ) ) ;
#21813 = CARTESIAN_POINT ( 'NONE',  ( -69.00000000109247367, 7.933012699999995476, 15.85617417291294196 ) ) ;
#21814 = DIRECTION ( 'NONE',  ( 0.000000000000000000, 0.000000000000000000, 1.000000000000000000 ) ) ;
#21815 = LINE ( 'NONE', #3381, #3261 ) ;
#21816 = ORIENTED_EDGE ( 'NONE', *, *, #16088, .T. ) ;
#21817 = AXIS2_PLACEMENT_3D ( 'NONE', #22764, #8646, #4921 ) ;
#21818 = AXIS2_PLACEMENT_3D ( 'NONE', #7072, #6713, #3344 ) ;
#21819 = ORIENTED_EDGE ( 'NONE', *, *, #7889, .T. ) ;
#21820 = LINE ( 'NONE', #30, #16734 ) ;
#21821 = CARTESIAN_POINT ( 'NONE',  ( 50.93981816583844591, 10.06805114094563791, 17.99999999999999645 ) ) ;
#21822 = CARTESIAN_POINT ( 'NONE',  ( -69.65000000109247935, 9.999999999999998224, 17.06698730000000097 ) ) ;
#21823 = CARTESIAN_POINT ( 'NONE',  ( -70.30000000109248504, 10.85617417291294551, 12.93301269999999370 ) ) ;
#21824 = CARTESIAN_POINT ( 'NONE',  ( 1.432654583217643163, -3.458734124999999882, 11.00000000136560452 ) ) ;
#21825 = CARTESIAN_POINT ( 'NONE',  ( 2.828427124746191179, 2.828427124746190291, 11.75000000273119660 ) ) ;
#21826 = CARTESIAN_POINT ( 'NONE',  ( 54.84375000000000000, 8.757359312880723223, 18.00000000000000355 ) ) ;
#21827 = CIRCLE ( 'NONE', #16111, 1.000000000000002665 ) ;
#21828 = PLANE ( 'NONE',  #11412 ) ;
#21829 = EDGE_CURVE ( 'NONE', #4570, #21012, #11493, .T. ) ;
#21830 = CARTESIAN_POINT ( 'NONE',  ( 52.31250000000000711, 13.00000000000000000, 14.99999999999998757 ) ) ;
#21831 = CARTESIAN_POINT ( 'NONE',  ( -1.101472369599993062, -3.286364942703593695, 2.039999999999997371 ) ) ;
#21832 = ADVANCED_FACE ( 'NONE', ( #13983 ), #12194, .F. ) ;
#21833 = FACE_OUTER_BOUND ( 'NONE', #20942, .T. ) ;
#21834 = EDGE_CURVE ( 'NONE', #22990, #4495, #17581, .T. ) ;
#21835 = ORIENTED_EDGE ( 'NONE', *, *, #20614, .T. ) ;
#21836 = CARTESIAN_POINT ( 'NONE',  ( 70.05000000218494449, 12.50000000000000000, 16.03553390593273775 ) ) ;
#21837 = CARTESIAN_POINT ( 'NONE',  ( -70.20000000000000284, 8.232233047033627571, 16.76776695296636532 ) ) ;
#21838 = EDGE_LOOP ( 'NONE', ( #8533, #17353, #10018 ) ) ;
#21839 = CARTESIAN_POINT ( 'NONE',  ( 53.62500000000000711, 12.12132034355964727, 17.12132034355963484 ) ) ;
#21840 = CARTESIAN_POINT ( 'NONE',  ( 1.656854249492380360, 4.000000000000000000, -2.887499997268812457 ) ) ;
#21841 = CARTESIAN_POINT ( 'NONE',  ( -90.00000000000000000, 0.000000000000000000, -6.000000000000021316 ) ) ;
#21842 = EDGE_LOOP ( 'NONE', ( #8783, #2665, #17538, #12511 ) ) ;
#21843 = CARTESIAN_POINT ( 'NONE',  ( -2.828427124746189403, 2.828427124746190291, 18.87500000000001066 ) ) ;
#21844 = CARTESIAN_POINT ( 'NONE',  ( 4.999999999999999112, 0.000000000000000000, 0.000000000000000000 ) ) ;
#21845 = DIRECTION ( 'NONE',  ( -1.000000000000000000, -0.000000000000000000, -0.000000000000000000 ) ) ;
#21846 = ORIENTED_EDGE ( 'NONE', *, *, #16484, .T. ) ;
#21847 = DIRECTION ( 'NONE',  ( -1.224646799147353207E-16, 0.000000000000000000, -1.000000000000000000 ) ) ;
#21848 = CARTESIAN_POINT ( 'NONE',  ( 4.999999999999999112, 0.000000000000000000, 0.000000000000000000 ) ) ;
#21849 = CARTESIAN_POINT ( 'NONE',  ( 72.14999999999999147, 11.03553390593273598, 12.49999999999999289 ) ) ;
#21850 = DIRECTION ( 'NONE',  ( -0.9396926207859107594, -0.3420201433256623291, 1.540743955509804830E-32 ) ) ;
#21851 = CARTESIAN_POINT ( 'NONE',  ( 69.34999999999999432, 8.964466094067214286, 17.49999999999996092 ) ) ;
#21852 = ADVANCED_FACE ( 'NONE', ( #3296 ), #7141, .F. ) ;
#21853 = CARTESIAN_POINT ( 'NONE',  ( 52.90856816583843880, 13.97181229448534978, 13.27509460956196641 ) ) ;
#21854 = CARTESIAN_POINT ( 'NONE',  ( 2.445694354108820079, 2.445694354108820523, -1.637499998634403209 ) ) ;
#21855 = CARTESIAN_POINT ( 'NONE',  ( 4.999999999999999112, 0.000000000000000000, 0.000000000000000000 ) ) ;
#21856 = DIRECTION ( 'NONE',  ( 0.000000000000000000, 1.000000000000000000, -1.224646799147353207E-16 ) ) ;
#21857 = FACE_OUTER_BOUND ( 'NONE', #22129, .T. ) ;
#21858 = ORIENTED_EDGE ( 'NONE', *, *, #14808, .F. ) ;
#21859 = CARTESIAN_POINT ( 'NONE',  ( 4.000000000000000888, 4.898587196589412829E-16, 11.62500000273119660 ) ) ;
#21860 = CARTESIAN_POINT ( 'NONE',  ( 69.29999999999999716, 9.999999999999998224, 17.49999999999999645 ) ) ;
#21861 = LINE ( 'NONE', #8975, #23116 ) ;
#21862 = ORIENTED_EDGE ( 'NONE', *, *, #20199, .T. ) ;
#21863 = ORIENTED_EDGE ( 'NONE', *, *, #11733, .F. ) ;
#21864 = CARTESIAN_POINT ( 'NONE',  ( 4.999999999999999112, 8.475820894092974456, 4.057423117305423155 ) ) ;
#21865 = ORIENTED_EDGE ( 'NONE', *, *, #16675, .F. ) ;
#21866 = CARTESIAN_POINT ( 'NONE',  ( 54.18750000000000711, 9.999999999999978684, 10.99999999999999645 ) ) ;
#21867 = VERTEX_POINT ( 'NONE', #14225 ) ;
#21868 = CARTESIAN_POINT ( 'NONE',  ( 1.971781867644420635E-15, -4.000000000000000000, 18.25000000000001066 ) ) ;
#21869 = VERTEX_POINT ( 'NONE', #12313 ) ;
#21870 = CARTESIAN_POINT ( 'NONE',  ( 53.18981816583844591, 9.931948859054346102, 10.99999999999999467 ) ) ;
#21871 = AXIS2_PLACEMENT_3D ( 'NONE', #13530, #18788, #15453 ) ;
#21872 = CARTESIAN_POINT ( 'NONE',  ( 68.25000000218494733, 11.03553390593273598, 12.49999999999999289 ) ) ;
#21873 = CARTESIAN_POINT ( 'NONE',  ( -19.99999999999999645, -9.000000000000003553, 10.00000000000008882 ) ) ;
#21874 = CARTESIAN_POINT ( 'NONE',  ( -68.70000000000000284, 7.499999999999996447, 14.99999999999999645 ) ) ;
#21875 = CARTESIAN_POINT ( 'NONE',  ( 54.99999999999992895, -15.00000000000000000, 1.836970198721037478E-15 ) ) ;
#21876 = ORIENTED_EDGE ( 'NONE', *, *, #20915, .F. ) ;
#21877 = CARTESIAN_POINT ( 'NONE',  ( 4.000000000000001776, -1.656854249492379694, 16.56250000273119838 ) ) ;
#21878 = CARTESIAN_POINT ( 'NONE',  ( -90.00000000000000000, 0.000000000000000000, -6.735000000000022524 ) ) ;
#21879 = CARTESIAN_POINT ( 'NONE',  ( 59.21643183416158962, 13.97181229448536399, 16.72490539043799629 ) ) ;
#21880 = PLANE ( 'NONE',  #21049 ) ;
#21881 = DIRECTION ( 'NONE',  ( 0.000000000000000000, 0.000000000000000000, 1.000000000000000000 ) ) ;
#21882 = CARTESIAN_POINT ( 'NONE',  ( 72.09999999999999432, 9.999999999999998224, 12.49999999999999289 ) ) ;
#21883 = CARTESIAN_POINT ( 'NONE',  ( 4.197310751797292738, 0.8178363989516252985, -3.502498386812444409 ) ) ;
#21884 = ORIENTED_EDGE ( 'NONE', *, *, #1429, .T. ) ;
#21885 = DIRECTION ( 'NONE',  ( 0.000000000000000000, 0.000000000000000000, 1.000000000000000000 ) ) ;
#21886 = CARTESIAN_POINT ( 'NONE',  ( 55.21875000000000711, 13.00000000000000533, 16.24264068711927322 ) ) ;
#21887 = CARTESIAN_POINT ( 'NONE',  ( -20.00000000000001066, 9.999999999999964473, -49.99999999999999289 ) ) ;
#21888 = DIRECTION ( 'NONE',  ( 1.000000000000000000, 0.000000000000000000, 0.000000000000000000 ) ) ;
#21889 = VERTEX_POINT ( 'NONE', #15670 ) ;
#21890 = CARTESIAN_POINT ( 'NONE',  ( -3.019423509283438722, -8.974600000000002353, 5.000000000000079936 ) ) ;
#21891 = CARTESIAN_POINT ( 'NONE',  ( 2.445694354108820079, 2.445694354108820523, -1.637499998634403209 ) ) ;
#21892 = DIRECTION ( 'NONE',  ( 0.000000000000000000, 0.000000000000000000, 1.000000000000000000 ) ) ;
#21893 = ORIENTED_EDGE ( 'NONE', *, *, #2960, .F. ) ;
#21894 = FACE_OUTER_BOUND ( 'NONE', #7758, .T. ) ;
#21895 = ORIENTED_EDGE ( 'NONE', *, *, #21930, .F. ) ;
#21896 = ADVANCED_FACE ( 'NONE', ( #1136 ), #17913, .T. ) ;
#21897 = DIRECTION ( 'NONE',  ( -1.000000000000000000, -0.000000000000000000, -0.000000000000000000 ) ) ;
#21898 = CARTESIAN_POINT ( 'NONE',  ( -2.828427124746189403, 2.828427124746190291, 16.87500000000001066 ) ) ;
#21899 = CARTESIAN_POINT ( 'NONE',  ( 27.50000000000000000, 7.500000000000001776, -36.31025403784445871 ) ) ;
#21900 = CARTESIAN_POINT ( 'NONE',  ( 46.41788101966725577, -11.25000000000000355, 10.00000000000008882 ) ) ;
#21901 = CARTESIAN_POINT ( 'NONE',  ( 11.86036186966726191, -11.25000000000000355, 10.00000000000008882 ) ) ;
#21902 = ADVANCED_FACE ( 'NONE', ( #6556, #13750 ), #13872, .T. ) ;
#21903 = ORIENTED_EDGE ( 'NONE', *, *, #2709, .T. ) ;
#21904 = CARTESIAN_POINT ( 'NONE',  ( -66.94999999999998863, 8.964466094067258695, 17.50000000000000355 ) ) ;
#21905 = DIRECTION ( 'NONE',  ( 1.224646799147353207E-16, -0.000000000000000000, 1.000000000000000000 ) ) ;
#21906 = CARTESIAN_POINT ( 'NONE',  ( 72.00000000109245946, 12.06698730000000275, 14.14382582708705094 ) ) ;
#21907 = CARTESIAN_POINT ( 'NONE',  ( 1.432654583217641164, 3.458734125000000326, 16.12500000136560629 ) ) ;
#21908 = CARTESIAN_POINT ( 'NONE',  ( -1.240299975428134203E-15, -4.736529461165891242, -3.681130640444276292 ) ) ;
#21909 = B_SPLINE_CURVE_WITH_KNOTS ( 'NONE', 3,
 ( #20580, #9474, #6226, #352, #13310, #8037 ),
 .UNSPECIFIED., .F., .F.,
 ( 4, 2, 4 ),
 ( 2.380733003127974818E-07, 0.001898835937927380270, 0.003797433802554448044 ),
 .UNSPECIFIED. ) ;
#21910 = CARTESIAN_POINT ( 'NONE',  ( -2.445694354108819635, -2.445694354108820967, -2.887499998634404097 ) ) ;
#21911 = CARTESIAN_POINT ( 'NONE',  ( -1.432654583217639610, -3.458734124999999882, 13.62500000136560452 ) ) ;
#21912 = DIRECTION ( 'NONE',  ( 0.000000000000000000, 1.000000000000000000, -1.224646799147353207E-16 ) ) ;
#21913 = ORIENTED_EDGE ( 'NONE', *, *, #7439, .T. ) ;
#21914 = CARTESIAN_POINT ( 'NONE',  ( -70.15000000109247935, 11.46158073645647235, 13.53841926354352232 ) ) ;
#21915 = VERTEX_POINT ( 'NONE', #10283 ) ;
#21916 = CARTESIAN_POINT ( 'NONE',  ( 53.77893183416158251, 8.411196891453236901, 10.97181229448535511 ) ) ;
#21917 = CARTESIAN_POINT ( 'NONE',  ( -71.05000000109245661, 9.999999999999998224, 12.93301269999999192 ) ) ;
#21918 = DIRECTION ( 'NONE',  ( 0.000000000000000000, 0.000000000000000000, 1.000000000000000000 ) ) ;
#21919 = DIRECTION ( 'NONE',  ( 1.000000000000000000, 7.703719777548943412E-32, 0.000000000000000000 ) ) ;
#21920 = EDGE_LOOP ( 'NONE', ( #22522, #5036, #7162, #20907 ) ) ;
#21921 = VECTOR ( 'NONE', #20521, 1000.000000000000000 ) ;
#21922 = EDGE_CURVE ( 'NONE', #476, #22239, #21013, .T. ) ;
#21923 = ADVANCED_FACE ( 'NONE', ( #23295 ), #6670, .F. ) ;
#21924 = ORIENTED_EDGE ( 'NONE', *, *, #19443, .F. ) ;
#21925 = DIRECTION ( 'NONE',  ( 1.000000000000000000, 0.000000000000000000, 0.000000000000000000 ) ) ;
#21926 = CARTESIAN_POINT ( 'NONE',  ( 54.59606816583844591, 11.17458954617364242, 11.97181229448534800 ) ) ;
#21927 = CARTESIAN_POINT ( 'NONE',  ( -71.10000000109246798, 12.06698730000000275, 15.85617417291294196 ) ) ;
#21928 = EDGE_CURVE ( 'NONE', #16967, #18422, #21244, .T. ) ;
#21929 = MANIFOLD_SOLID_BREP ( 'M5 Clearance Hole1', #20396 ) ;
#21930 = EDGE_CURVE ( 'NONE', #4420, #16525, #3757, .T. ) ;
#21931 = CARTESIAN_POINT ( 'NONE',  ( -69.95000000109247651, 8.538419263543522320, 16.46158073645647235 ) ) ;
#21932 =( BOUNDED_CURVE ( )  B_SPLINE_CURVE ( 2, ( #18020, #23400, #7006, #10747, #1355, #12411, #15994, #21467, #23279 ),
 .UNSPECIFIED., .F., .F. ) 
 B_SPLINE_CURVE_WITH_KNOTS ( ( 3, 2, 2, 2, 3 ),
 ( 0.1875000000000010270, 0.2031250000000009437, 0.2187500000000008327, 0.2343750000000007494, 0.2500000000000006661 ),
 .UNSPECIFIED. ) 
 CURVE ( )  GEOMETRIC_REPRESENTATION_ITEM ( )  RATIONAL_B_SPLINE_CURVE ( ( 0.9999999999999950040, 0.9238795325112917345, 1.000000000000000000, 0.9238795325112867385, 1.000000000000000000, 0.9238795325112867385, 1.000000000000000000, 0.9238795325112835188, 1.000000000000003331 ) ) 
 REPRESENTATION_ITEM ( '' )  );
#21933 = CARTESIAN_POINT ( 'NONE',  ( 3.458734125000001658, 4.235727675282972223E-16, 11.18750000136560452 ) ) ;
#21934 = CARTESIAN_POINT ( 'NONE',  ( -19.99999999999999645, -9.000000000000003553, 10.00000000000008882 ) ) ;
#21935 = CARTESIAN_POINT ( 'NONE',  ( 53.25000000000000711, 7.878679656440361612, 17.12132034355964549 ) ) ;
#21936 = LINE ( 'NONE', #16689, #17730 ) ;
#21937 = CARTESIAN_POINT ( 'NONE',  ( 54.65625000000001421, 7.000000000000003553, 16.24264068711929099 ) ) ;
#21938 = CARTESIAN_POINT ( 'NONE',  ( -1.656854249492380138, -3.999999999999999112, 16.31250000273119483 ) ) ;
#21939 = CARTESIAN_POINT ( 'NONE',  ( -3.458734124999998993, 0.000000000000000000, 19.56250000136560629 ) ) ;
#21940 = ORIENTED_EDGE ( 'NONE', *, *, #23679, .F. ) ;
#21941 = CARTESIAN_POINT ( 'NONE',  ( 70.00000000218494733, 12.50000000000000000, 14.99999999999999645 ) ) ;
#21942 = LINE ( 'NONE', #22300, #23502 ) ;
#21943 = VERTEX_POINT ( 'NONE', #6780 ) ;
#21944 = CARTESIAN_POINT ( 'NONE',  ( 53.43750000000000711, 10.00000000000000711, 17.99999999999999645 ) ) ;
#21945 = CARTESIAN_POINT ( 'NONE',  ( 7.347880794884118750E-16, -4.000000000000000000, -3.324999997268812901 ) ) ;
#21946 = DIRECTION ( 'NONE',  ( 0.3420201433256622736, 0.9396926207859106484, 0.000000000000000000 ) ) ;
#21947 = EDGE_LOOP ( 'NONE', ( #21442, #15630, #412, #10556 ) ) ;
#21948 = CARTESIAN_POINT ( 'NONE',  ( 4.000000000000000888, 1.656854249492381248, 17.56250000000001421 ) ) ;
#21949 = CARTESIAN_POINT ( 'NONE',  ( -1.656854249492381248, -3.999999999999999112, -2.512499999999998845 ) ) ;
#21950 = AXIS2_PLACEMENT_3D ( 'NONE', #8493, #13883, #6328 ) ;
#21951 = ADVANCED_FACE ( 'NONE', ( #3418 ), #18381, .F. ) ;
#21952 = CARTESIAN_POINT ( 'NONE',  ( 68.89999999999999147, 9.999999999999998224, 12.49999999999999289 ) ) ;
#21953 = EDGE_LOOP ( 'NONE', ( #1101, #19150, #17182, #1021 ) ) ;
#21954 = CARTESIAN_POINT ( 'NONE',  ( 15.00195451966726523, -11.25000000000000355, 10.00000000000008882 ) ) ;
#21955 = CARTESIAN_POINT ( 'NONE',  ( -3.270501301980698550, -1.125461230421587633, 2.040000000000001812 ) ) ;
#21956 = ADVANCED_FACE ( 'NONE', ( #1841 ), #10760, .F. ) ;
#21957 = CARTESIAN_POINT ( 'NONE',  ( 67.70000000000000284, 9.999999999999998224, 17.49999999999999645 ) ) ;
#21958 = CARTESIAN_POINT ( 'NONE',  ( -18.13102059071655248, -8.974600000000002353, 5.000000000000079936 ) ) ;
#21959 = VECTOR ( 'NONE', #8757, 1000.000000000000000 ) ;
#21961 = DIRECTION ( 'NONE',  ( 0.000000000000000000, 0.5877852522924742473, -0.8090169943749466741 ) ) ;
#21960 = VECTOR ( 'NONE', #4972, 1000.000000000000000 ) ;
#21962 = CARTESIAN_POINT ( 'NONE',  ( 54.03356816583844591, 11.72490539043803004, 18.97181229448534268 ) ) ;
#21963 = VECTOR ( 'NONE', #7661, 1000.000000000000000 ) ;
#21964 = CARTESIAN_POINT ( 'NONE',  ( -3.458734124999999882, -1.432654583217642497, -1.199999998634403431 ) ) ;
#21965 = CARTESIAN_POINT ( 'NONE',  ( -2.445694354108819191, 2.445694354108820523, 19.56250000136560629 ) ) ;
#21966 = DIRECTION ( 'NONE',  ( 0.000000000000000000, 1.000000000000000000, 3.469446951953611822E-15 ) ) ;
#21967 = CARTESIAN_POINT ( 'NONE',  ( -2.828427124746190291, 2.828427124746190291, 0.1750000000000015432 ) ) ;
#21968 = CARTESIAN_POINT ( 'NONE',  ( -11.01965741966725076, -11.25000000000000355, 5.000000000000079936 ) ) ;
#21969 = ORIENTED_EDGE ( 'NONE', *, *, #18011, .T. ) ;
#21970 = CARTESIAN_POINT ( 'NONE',  ( 5.000000000000000888, 4.898587196589412829E-16, -4.000000000000000000 ) ) ;
#21971 = DIRECTION ( 'NONE',  ( -1.000000000000000000, -0.000000000000000000, -0.000000000000000000 ) ) ;
#21972 = CARTESIAN_POINT ( 'NONE',  ( -19.99999999999999645, -9.000000000000003553, 5.000000000000079936 ) ) ;
#21973 = ORIENTED_EDGE ( 'NONE', *, *, #7765, .T. ) ;
#21974 = ORIENTED_EDGE ( 'NONE', *, *, #15774, .T. ) ;
#21975 = DIRECTION ( 'NONE',  ( -1.000000000000000000, -0.000000000000000000, -0.000000000000000000 ) ) ;
#21976 = VERTEX_POINT ( 'NONE', #1611 ) ;
#21977 = CARTESIAN_POINT ( 'NONE',  ( 55.21875000000000711, 14.00000000000001066, 16.65685424949235482 ) ) ;
#21978 = ORIENTED_EDGE ( 'NONE', *, *, #12379, .F. ) ;
#21979 = DIRECTION ( 'NONE',  ( -0.5000000000000051070, 1.060575238724903217E-16, -0.8660254037844355990 ) ) ;
#21980 = ORIENTED_EDGE ( 'NONE', *, *, #4066, .F. ) ;
#21981 = CARTESIAN_POINT ( 'NONE',  ( 52.72106816583844591, 14.02818770551465377, 16.58880310854672757 ) ) ;
#21982 = VECTOR ( 'NONE', #6336, 1000.000000000000000 ) ;
#21983 = AXIS2_PLACEMENT_3D ( 'NONE', #11376, #15207, #6082 ) ;
#21984 = EDGE_CURVE ( 'NONE', #17502, #10342, #55, .T. ) ;
#21985 = CARTESIAN_POINT ( 'NONE',  ( 71.65000000109247935, 9.999999999999998224, 12.93301269999999192 ) ) ;
#21986 = CARTESIAN_POINT ( 'NONE',  ( 4.999999999999999112, 0.000000000000000000, 0.000000000000000000 ) ) ;
#21987 = LINE ( 'NONE', #22463, #284 ) ;
#21988 = CARTESIAN_POINT ( 'NONE',  ( 65.00000000000000000, -10.00000000000000178, 14.99999999999999467 ) ) ;
#21989 = VERTEX_POINT ( 'NONE', #18035 ) ;
#21990 = CARTESIAN_POINT ( 'NONE',  ( 1.656854249492384135, -3.999999999999999112, 16.43750000273119838 ) ) ;
#21991 = CARTESIAN_POINT ( 'NONE',  ( 5.000000000000002665, 0.000000000000000000, -2.700000000000000622 ) ) ;
#21992 = CARTESIAN_POINT ( 'NONE',  ( 55.74768183416157541, 7.123453452023678523, 17.78030770151605822 ) ) ;
#21993 = CARTESIAN_POINT ( 'NONE',  ( 1.876855952934447513, -6.421950209808290566, -3.593844378834461395 ) ) ;
#21994 = FACE_OUTER_BOUND ( 'NONE', #12513, .T. ) ;
#21995 = CARTESIAN_POINT ( 'NONE',  ( 27.50000000000000000, 7.500000000000002665, -31.01025403784447576 ) ) ;
#21996 = AXIS2_PLACEMENT_3D ( 'NONE', #19545, #14187, #16208 ) ;
#21997 = LINE ( 'NONE', #3683, #7300 ) ;
#21998 = VERTEX_POINT ( 'NONE', #18145 ) ;
#21999 = DIRECTION ( 'NONE',  ( -0.5000000000000019984, -0.8660254037844375974, 0.000000000000000000 ) ) ;
#22000 = CARTESIAN_POINT ( 'NONE',  ( -4.000000000000000000, 1.700094919196744270, -3.320312364301766017 ) ) ;
#22001 = VECTOR ( 'NONE', #12569, 1000.000000000000000 ) ;
#22002 = DIRECTION ( 'NONE',  ( -1.000000000000000000, 0.000000000000000000, -0.000000000000000000 ) ) ;
#22003 =( NAMED_UNIT ( * ) SI_UNIT ( $, .STERADIAN. ) SOLID_ANGLE_UNIT ( ) );
#22004 = VERTEX_POINT ( 'NONE', #7388 ) ;
#22005 = CARTESIAN_POINT ( 'NONE',  ( 1.506022603841227436, 0.000000000000000000, 0.000000000000000000 ) ) ;
#22006 = CARTESIAN_POINT ( 'NONE',  ( -6.161016159283438931, -8.974600000000002353, 10.00000000000008882 ) ) ;
#22007 = CARTESIAN_POINT ( 'NONE',  ( 0.6920835326022565237, 4.454600218803884459, -3.597382984111579862 ) ) ;
#22008 = ORIENTED_EDGE ( 'NONE', *, *, #9929, .T. ) ;
#22009 = ORIENTED_EDGE ( 'NONE', *, *, #4832, .F. ) ;
#22010 = CARTESIAN_POINT ( 'NONE',  ( -2.828427124746189403, 2.828427124746190291, 19.00000000273119838 ) ) ;
#22011 = CARTESIAN_POINT ( 'NONE',  ( 4.000000000000001776, -1.656854249492379694, 18.43750000000000711 ) ) ;
#22012 = CARTESIAN_POINT ( 'NONE',  ( 22.71892870323381075, -9.000000000000005329, 10.00000000000008882 ) ) ;
#22013 = CARTESIAN_POINT ( 'NONE',  ( 27.50000000000000000, 1.500000000000003109, -33.66025403784446723 ) ) ;
#22014 = LINE ( 'NONE', #6993, #9872 ) ;
#22015 =( NAMED_UNIT ( * ) SI_UNIT ( $, .STERADIAN. ) SOLID_ANGLE_UNIT ( ) );
#22016 = ORIENTED_EDGE ( 'NONE', *, *, #5765, .T. ) ;
#22017 = LINE ( 'NONE', #7564, #3387 ) ;
#22018 = CARTESIAN_POINT ( 'NONE',  ( -4.000000000000000000, 0.000000000000000000, -0.5749999972688123462 ) ) ;
#22019 = CARTESIAN_POINT ( 'NONE',  ( 67.70000000109246230, 10.85617417291294551, 12.93301269999999370 ) ) ;
#22020 = CARTESIAN_POINT ( 'NONE',  ( -3.458734124999998993, 0.000000000000000000, 18.43750000136560629 ) ) ;
#22021 = DIRECTION ( 'NONE',  ( 0.000000000000000000, -0.3090169943749350168, -0.9510565162951576390 ) ) ;
#22022 = EDGE_CURVE ( 'NONE', #13240, #3850, #8954, .T. ) ;
#22023 = CARTESIAN_POINT ( 'NONE',  ( 2.828427124746190735, -2.828427124746189847, 4.675000000000000711 ) ) ;
#22024 = DIRECTION ( 'NONE',  ( -1.000000000000000000, 0.000000000000000000, 1.224646799147352961E-16 ) ) ;
#22025 = CARTESIAN_POINT ( 'NONE',  ( -3.458734124999998993, -1.432654583217642497, 14.50000000136560629 ) ) ;
#22026 = VERTEX_POINT ( 'NONE', #9066 ) ;
#22027 = CARTESIAN_POINT ( 'NONE',  ( -67.50000000109247367, 7.933012699999995476, 14.14382582708705094 ) ) ;
#22028 = ORIENTED_EDGE ( 'NONE', *, *, #18888, .F. ) ;
#22029 = CARTESIAN_POINT ( 'NONE',  ( 57.52893183416158962, 11.58880310854676132, 19.02818770551463956 ) ) ;
#22030 = CARTESIAN_POINT ( 'NONE',  ( -70.90000000109245093, 7.933012699999995476, 14.14382582708705094 ) ) ;
#22031 = ITEM_DEFINED_TRANSFORMATION ( 'NONE', 'NONE', #20488,  #7318 ) ;
#22032 = EDGE_CURVE ( 'NONE', #5149, #22090, #9302, .T. ) ;
#22033 = CARTESIAN_POINT ( 'NONE',  ( -2.828427124746188515, -2.828427124746190735, 17.12500000000001066 ) ) ;
#22034 = ORIENTED_EDGE ( 'NONE', *, *, #22228, .F. ) ;
#22035 = ORIENTED_EDGE ( 'NONE', *, *, #11284, .T. ) ;
#22036 = CARTESIAN_POINT ( 'NONE',  ( 2.445694354108822299, -2.445694354108820079, 19.06250000136560629 ) ) ;
#22037 = CARTESIAN_POINT ( 'NONE',  ( 53.56481816583844591, 6.999999999999998224, 15.06805114094563436 ) ) ;
#22038 = CARTESIAN_POINT ( 'NONE',  ( -70.25000000109247367, 12.06698730000000097, 14.99999999999999645 ) ) ;
#22039 = CIRCLE ( 'NONE', #8320, 8.800000000000022027 ) ;
#22040 = CARTESIAN_POINT ( 'NONE',  ( -70.40000000109247935, 12.06698730000000275, 14.14382582708705094 ) ) ;
#22041 = CARTESIAN_POINT ( 'NONE',  ( 2.445694354108822299, -2.445694354108820079, 13.06250000136560629 ) ) ;
#22042 = CARTESIAN_POINT ( 'NONE',  ( -1.799999999999996048, 0.000000000000000000, 0.000000000000000000 ) ) ;
#22043 = CARTESIAN_POINT ( 'NONE',  ( 51.65625000000000711, 7.000000000000003553, 16.24264068711929099 ) ) ;
#22044 = FACE_OUTER_BOUND ( 'NONE', #8159, .T. ) ;
#22045 = ADVANCED_FACE ( 'NONE', ( #23417, #7021, #23654 ), #1725, .T. ) ;
#22046 = CARTESIAN_POINT ( 'NONE',  ( 51.65625000000000711, 7.000000000000003553, 16.24264068711929099 ) ) ;
#22047 = EDGE_CURVE ( 'NONE', #12818, #1359, #16431, .T. ) ;
#22048 = CARTESIAN_POINT ( 'NONE',  ( 1.656854249492381470, 4.000000000000000000, 15.81250000273119660 ) ) ;
#22049 = VECTOR ( 'NONE', #2374, 1000.000000000000000 ) ;
#22050 = AXIS2_PLACEMENT_3D ( 'NONE', #10223, #21302, #14166 ) ;
#22051 = ORIENTED_EDGE ( 'NONE', *, *, #19552, .F. ) ;
#22052 = CARTESIAN_POINT ( 'NONE',  ( 65.00000000000000000, 15.00000000000000000, 19.99999999999999645 ) ) ;
#22053 = CARTESIAN_POINT ( 'NONE',  ( -70.29999999999999716, 7.499999999999996447, 14.99999999999999645 ) ) ;
#22054 = EDGE_LOOP ( 'NONE', ( #14927, #6096, #16242, #5823, #13743, #8282, #23350, #13802, #18870, #8042, #13657, #8126, #5941, #13107, #16605, #1776, #1166, #22051, #23573, #15041, #9917, #6190, #21738, #19773 ) ) ;
#22055 = CARTESIAN_POINT ( 'NONE',  ( 51.75000000000000711, 7.878679656440361612, 17.12132034355964549 ) ) ;
#22056 = CARTESIAN_POINT ( 'NONE',  ( -3.458734125000000326, 0.000000000000000000, 5.737500001365596347 ) ) ;
#22057 = ADVANCED_FACE ( 'NONE', ( #14456, #5212 ), #12678, .T. ) ;
#22058 = FACE_OUTER_BOUND ( 'NONE', #13783, .T. ) ;
#22059 = ORIENTED_EDGE ( 'NONE', *, *, #8964, .T. ) ;
#22060 = CARTESIAN_POINT ( 'NONE',  ( 4.000000000000000888, 1.656854249492381248, 18.56250000000001421 ) ) ;
#22061 = LINE ( 'NONE', #1838, #1446 ) ;
#22062 = FACE_OUTER_BOUND ( 'NONE', #1333, .T. ) ;
#22063 = EDGE_LOOP ( 'NONE', ( #19167, #15277, #7551, #9052 ) ) ;
#22064 = VECTOR ( 'NONE', #6172, 1000.000000000000000 ) ;
#22065 = LINE ( 'NONE', #1843, #14441 ) ;
#22066 =( BOUNDED_SURFACE ( )  B_SPLINE_SURFACE ( 1, 2, ( 
 ( #11601, #6307, #789, #9914, #13508, #542, #895, #13394, #657, #20661, #12071, #11716, #22812, #2342, #17449, #17330, #7866, #4379, #18868, #15188, #13865, #2453, #9788, #22585, #17084, #17211, #13623, #7991, #8346, #21007, #4494, #19111, #11835, #18982, #4624, #11958, #15313, #6188, #2700, #10156, #8230, #15547, #6424, #22448, #20773, #13741, #4739, #15664, #6061, #22937, #21123, #6550, #23407, #5084, #3053, #10630, #19806, #21591, #18027, #8475, #3408, #15780, #17679, #1483, #5204, #21354, #16001, #6664, #17906, #14329, #5325, #23286, #21237, #21713, #10274, #14448, #23522, #7134, #13977, #17565, #1243, #12418, #4849, #12184, #8697, #19684, #16234, #17791, #8826, #12544, #14216, #15886, #10753, #1602, #1130, #16123, #1361, #19336, #23051, #6896, #7012, #21474, #2924, #19456, #8943, #10399, #8581, #19569, #23164, #6774, #14090, #4976, #12307, #3164, #10510, #3289, #13008, #9528, #22304, #406, #7259, #18484, #12777, #16826, #16349, #12887, #5556, #9293, #14688, #3526, #18374, #20144, #19926, #21840, #11210, #16470, #2191, #7733, #20387, #10972, #21945, #18136, #7491, #9058, #161, #2067, #14576, #47, #18248 ),
 ( #22056, #7381, #15046, #5442, #14807, #5674, #1716, #10859, #9408, #12670, #20030, #23645, #3993, #13127, #3633, #3748, #16698, #11089, #20273, #1833, #9183, #11334, #1954, #16582, #3877, #274, #7609, #14932, #22186, #5799, #18605, #4114, #4240, #9652, #11453, #20510, #13593, #7840, #2541, #4466, #6161, #18843, #2670, #11575, #2318, #11688, #20745, #11807, #13483, #15163, #16942, #22422, #7962, #11930, #17415, #2782, #519, #4593, #18957, #9886, #631, #6391, #15281, #18729, #20631, #5916, #22554, #6036, #9759, #760, #19078, #13362, #13244, #17178, #4351, #2428, #8092, #13711, #22783, #17301, #20973, #10122, #984, #15402, #22665, #17059, #6276, #20860, #10013, #865, #8200, #15514, #19197, #8638, #15938, #9241, #8885, #19979, #23218, #14631, #7200, #5034, #1546, #1414, #6830, #11032, #17847, #8756, #19746, #14275, #23468, #19867, #16062, #5501, #23352, #5264, #10335, #12365, #21891, #16179, #10690, #9007, #17964, #20091, #6958, #7075, #23588, #10810, #1663, #21536, #12832, #10575, #3582, #5144, #19627, #12608, #14392, #5388, #21655, #12485, #3225, #3348, #3471, #3692, #18316, #1898, #18082, #14154, #16299 ) ),
 .UNSPECIFIED., .F., .F., .F. ) 
 B_SPLINE_SURFACE_WITH_KNOTS ( ( 2, 2 ),
 ( 3, 2, 2, 2, 2, 2, 2, 2, 2, 2, 2, 2, 2, 2, 2, 2, 2, 2, 2, 2, 2, 2, 2, 2, 2, 2, 2, 2, 2, 2, 2, 2, 2, 2, 2, 2, 2, 2, 2, 2, 2, 2, 2, 2, 2, 2, 2, 2, 2, 2, 2, 2, 2, 2, 2, 2, 2, 2, 2, 2, 2, 2, 2, 2, 2, 2, 2, 2, 2, 2, 2, 2, 2, 2, 3 ),
 ( 0.000000000000000000, 1.000000000000000000 ),
 ( 0.000000000000000000, 0.01250000000000000069, 0.02500000000000000139, 0.03749999999999999861, 0.05000000000000000278, 0.06250000000000000000, 0.07499999999999999722, 0.08749999999999999445, 0.1000000000000000056, 0.1125000000000000028, 0.1250000000000000000, 0.1375000000000000111, 0.1499999999999999944, 0.1625000000000000056, 0.1749999999999999889, 0.1875000000000000000, 0.2000000000000000111, 0.2124999999999999944, 0.2250000000000000056, 0.2374999999999999889, 0.2500000000000000000, 0.2625000000000000111, 0.2750000000000000222, 0.2874999999999999778, 0.2999999999999999889, 0.3125000000000000000, 0.3250000000000000111, 0.3375000000000000222, 0.3499999999999999778, 0.3624999999999999889, 0.3750000000000000000, 0.3875000000000000111, 0.4000000000000000222, 0.4124999999999999778, 0.4249999999999999889, 0.4375000000000000000, 0.4500000000000000111, 0.4625000000000000222, 0.4749999999999999778, 0.4874999999999999889, 0.5000000000000000000, 0.5124999999999999556, 0.5250000000000000222, 0.5374999999999999778, 0.5500000000000000444, 0.5625000000000000000, 0.5749999999999999556, 0.5875000000000000222, 0.5999999999999999778, 0.6125000000000000444, 0.6250000000000000000, 0.6374999999999999556, 0.6500000000000000222, 0.6624999999999999778, 0.6750000000000000444, 0.6875000000000000000, 0.6999999999999999556, 0.7125000000000000222, 0.7249999999999999778, 0.7375000000000000444, 0.7500000000000000000, 0.7624999999999999556, 0.7750000000000000222, 0.7874999999999999778, 0.8000000000000000444, 0.8125000000000000000, 0.8249999999999999556, 0.8375000000000000222, 0.8499999999999999778, 0.8625000000000000444, 0.8750000000000000000, 0.8874999999999999556, 0.9000000000000000222, 0.9124999999999999778, 0.9250000000000000444 ),
 .UNSPECIFIED. ) 
 GEOMETRIC_REPRESENTATION_ITEM ( )  RATIONAL_B_SPLINE_SURFACE ( (
 ( 1.000000000000000000, 0.9238795325112867385, 1.000000000000000000, 0.9238795325112867385, 1.000000000000000000, 0.9238795325112867385, 1.000000000000000000, 0.9238795325112867385, 1.000000000000000000, 0.9238795325112867385, 1.000000000000000000, 0.9238795325112867385, 1.000000000000000000, 0.9238795325112867385, 1.000000000000000000, 0.9238795325112867385, 1.000000000000000000, 0.9238795325112867385, 1.000000000000000000, 0.9238795325112867385, 1.000000000000000000, 0.9238795325112867385, 1.000000000000000000, 0.9238795325112867385, 1.000000000000000000, 0.9238795325112867385, 1.000000000000000000, 0.9238795325112867385, 1.000000000000000000, 0.9238795325112867385, 1.000000000000000000, 0.9238795325112867385, 1.000000000000000000, 0.9238795325112867385, 1.000000000000000000, 0.9238795325112867385, 1.000000000000000000, 0.9238795325112867385, 1.000000000000000000, 0.9238795325112867385, 1.000000000000000000, 0.9238795325112867385, 1.000000000000000000, 0.9238795325112867385, 1.000000000000000000, 0.9238795325112867385, 1.000000000000000000, 0.9238795325112867385, 1.000000000000000000, 0.9238795325112867385, 1.000000000000000000, 0.9238795325112867385, 1.000000000000000000, 0.9238795325112867385, 1.000000000000000000, 0.9238795325112867385, 1.000000000000000000, 0.9238795325112867385, 1.000000000000000000, 0.9238795325112867385, 1.000000000000000000, 0.9238795325112867385, 1.000000000000000000, 0.9238795325112867385, 1.000000000000000000, 0.9238795325112867385, 1.000000000000000000, 0.9238795325112867385, 1.000000000000000000, 0.9238795325112867385, 1.000000000000000000, 0.9238795325112867385, 1.000000000000000000, 0.9238795325112867385, 1.000000000000000000, 0.9238795325112867385, 1.000000000000000000, 0.9238795325112867385, 1.000000000000000000, 0.9238795325112867385, 1.000000000000000000, 0.9238795325112867385, 1.000000000000000000, 0.9238795325112867385, 1.000000000000000000, 0.9238795325112867385, 1.000000000000000000, 0.9238795325112867385, 1.000000000000000000, 0.9238795325112867385, 1.000000000000000000, 0.9238795325112867385, 1.000000000000000000, 0.9238795325112867385, 1.000000000000000000, 0.9238795325112867385, 1.000000000000000000, 0.9238795325112867385, 1.000000000000000000, 0.9238795325112867385, 1.000000000000000000, 0.9238795325112867385, 1.000000000000000000, 0.9238795325112867385, 1.000000000000000000, 0.9238795325112867385, 1.000000000000000000, 0.9238795325112867385, 1.000000000000000000, 0.9238795325112867385, 1.000000000000000000, 0.9238795325112867385, 1.000000000000000000, 0.9238795325112867385, 1.000000000000000000, 0.9238795325112867385, 1.000000000000000000, 0.9238795325112867385, 1.000000000000000000, 0.9238795325112867385, 1.000000000000000000, 0.9238795325112867385, 1.000000000000000000, 0.9238795325112867385, 1.000000000000000000, 0.9238795325112867385, 1.000000000000000000, 0.9238795325112867385, 1.000000000000000000, 0.9238795325112867385, 1.000000000000000000, 0.9238795325112867385, 1.000000000000000000, 0.9238795325112867385, 1.000000000000000000, 0.9238795325112867385, 1.000000000000000000, 0.9238795325112867385, 1.000000000000000000, 0.9238795325112867385, 1.000000000000000000, 0.9238795325112867385, 1.000000000000000000, 0.9238795325112867385, 1.000000000000000000, 0.9238795325112867385, 1.000000000000000000, 0.9238795325112867385, 1.000000000000000000),
 ( 1.000000000000000000, 0.9238795325112867385, 1.000000000000000000, 0.9238795325112867385, 1.000000000000000000, 0.9238795325112867385, 1.000000000000000000, 0.9238795325112867385, 1.000000000000000000, 0.9238795325112867385, 1.000000000000000000, 0.9238795325112867385, 1.000000000000000000, 0.9238795325112867385, 1.000000000000000000, 0.9238795325112867385, 1.000000000000000000, 0.9238795325112867385, 1.000000000000000000, 0.9238795325112867385, 1.000000000000000000, 0.9238795325112867385, 1.000000000000000000, 0.9238795325112867385, 1.000000000000000000, 0.9238795325112867385, 1.000000000000000000, 0.9238795325112867385, 1.000000000000000000, 0.9238795325112867385, 1.000000000000000000, 0.9238795325112867385, 1.000000000000000000, 0.9238795325112867385, 1.000000000000000000, 0.9238795325112867385, 1.000000000000000000, 0.9238795325112867385, 1.000000000000000000, 0.9238795325112867385, 1.000000000000000000, 0.9238795325112867385, 1.000000000000000000, 0.9238795325112867385, 1.000000000000000000, 0.9238795325112867385, 1.000000000000000000, 0.9238795325112867385, 1.000000000000000000, 0.9238795325112867385, 1.000000000000000000, 0.9238795325112867385, 1.000000000000000000, 0.9238795325112867385, 1.000000000000000000, 0.9238795325112867385, 1.000000000000000000, 0.9238795325112867385, 1.000000000000000000, 0.9238795325112867385, 1.000000000000000000, 0.9238795325112867385, 1.000000000000000000, 0.9238795325112867385, 1.000000000000000000, 0.9238795325112867385, 1.000000000000000000, 0.9238795325112867385, 1.000000000000000000, 0.9238795325112867385, 1.000000000000000000, 0.9238795325112867385, 1.000000000000000000, 0.9238795325112867385, 1.000000000000000000, 0.9238795325112867385, 1.000000000000000000, 0.9238795325112867385, 1.000000000000000000, 0.9238795325112867385, 1.000000000000000000, 0.9238795325112867385, 1.000000000000000000, 0.9238795325112867385, 1.000000000000000000, 0.9238795325112867385, 1.000000000000000000, 0.9238795325112867385, 1.000000000000000000, 0.9238795325112867385, 1.000000000000000000, 0.9238795325112867385, 1.000000000000000000, 0.9238795325112867385, 1.000000000000000000, 0.9238795325112867385, 1.000000000000000000, 0.9238795325112867385, 1.000000000000000000, 0.9238795325112867385, 1.000000000000000000, 0.9238795325112867385, 1.000000000000000000, 0.9238795325112867385, 1.000000000000000000, 0.9238795325112867385, 1.000000000000000000, 0.9238795325112867385, 1.000000000000000000, 0.9238795325112867385, 1.000000000000000000, 0.9238795325112867385, 1.000000000000000000, 0.9238795325112867385, 1.000000000000000000, 0.9238795325112867385, 1.000000000000000000, 0.9238795325112867385, 1.000000000000000000, 0.9238795325112867385, 1.000000000000000000, 0.9238795325112867385, 1.000000000000000000, 0.9238795325112867385, 1.000000000000000000, 0.9238795325112867385, 1.000000000000000000, 0.9238795325112867385, 1.000000000000000000, 0.9238795325112867385, 1.000000000000000000, 0.9238795325112867385, 1.000000000000000000, 0.9238795325112867385, 1.000000000000000000, 0.9238795325112867385, 1.000000000000000000, 0.9238795325112867385, 1.000000000000000000, 0.9238795325112867385, 1.000000000000000000, 0.9238795325112867385, 1.000000000000000000, 0.9238795325112867385, 1.000000000000000000, 0.9238795325112867385, 1.000000000000000000, 0.9238795325112867385, 1.000000000000000000) ) ) 
 REPRESENTATION_ITEM ( '' )  SURFACE ( )  );
#22067 = CARTESIAN_POINT ( 'NONE',  ( 2.445694354108820079, 2.445694354108820523, 1.612500001365596125 ) ) ;
#22068 = VECTOR ( 'NONE', #5826, 1000.000000000000000 ) ;
#22069 = VECTOR ( 'NONE', #11491, 1000.000000000000114 ) ;
#22070 = CARTESIAN_POINT ( 'NONE',  ( 68.89999999999999147, 9.999999999999998224, 12.49999999999999289 ) ) ;
#22071 = EDGE_CURVE ( 'NONE', #1297, #5303, #20152, .T. ) ;
#22072 = CARTESIAN_POINT ( 'NONE',  ( -10.13078668033273999, -11.25000000000000355, 10.00000000000008882 ) ) ;
#22073 = CARTESIAN_POINT ( 'NONE',  ( -67.20000000000000284, 8.232233047033629347, 13.23223304703362402 ) ) ;
#22074 = CARTESIAN_POINT ( 'NONE',  ( 50.65856816583843880, 6.028187705514649330, 16.72490539043803182 ) ) ;
#22075 = EDGE_CURVE ( 'NONE', #1035, #1856, #12507, .T. ) ;
#22076 = CARTESIAN_POINT ( 'NONE',  ( -2.445694354108819635, -2.445694354108820523, -0.1374999986344035974 ) ) ;
#22077 = CARTESIAN_POINT ( 'NONE',  ( 1.432654583217641386, 3.458734125000000770, 14.37500000136560452 ) ) ;
#22078 = CARTESIAN_POINT ( 'NONE',  ( -71.75000000000001421, 8.964466094067221391, 17.49999999999996447 ) ) ;
#22079 = LINE ( 'NONE', #18625, #1717 ) ;
#22080 = VECTOR ( 'NONE', #12464, 1000.000000000000000 ) ;
#22081 = DIRECTION ( 'NONE',  ( 0.000000000000000000, 0.000000000000000000, -1.000000000000000000 ) ) ;
#22082 = EDGE_LOOP ( 'NONE', ( #13974, #9944, #1600, #4119 ) ) ;
#22083 = DIRECTION ( 'NONE',  ( 1.000000000000000000, 0.000000000000000000, 0.000000000000000000 ) ) ;
#22084 = CARTESIAN_POINT ( 'NONE',  ( 1.317756351988342622, -3.857995168970215438, -0.04852650426602527628 ) ) ;
#22085 = DIRECTION ( 'NONE',  ( 0.000000000000000000, 0.000000000000000000, 1.000000000000000000 ) ) ;
#22086 = EDGE_CURVE ( 'NONE', #16067, #11987, #9603, .T. ) ;
#22087 = ORIENTED_EDGE ( 'NONE', *, *, #13779, .T. ) ;
#22088 = VECTOR ( 'NONE', #21242, 1000.000000000000000 ) ;
#22089 = EDGE_CURVE ( 'NONE', #21603, #1132, #3367, .T. ) ;
#22090 = VERTEX_POINT ( 'NONE', #6974 ) ;
#22091 = AXIS2_PLACEMENT_3D ( 'NONE', #19200, #13952, #15864 ) ;
#22092 = PLANE ( 'NONE',  #4878 ) ;
#22093 = CARTESIAN_POINT ( 'NONE',  ( 56.34375000000000711, 8.343145750507636293, 19.00000000000000000 ) ) ;
#22094 = ORIENTED_EDGE ( 'NONE', *, *, #18149, .F. ) ;
#22095 = DIRECTION ( 'NONE',  ( -1.000000000000000000, -0.000000000000000000, -0.000000000000000000 ) ) ;
#22096 = ORIENTED_EDGE ( 'NONE', *, *, #16815, .T. ) ;
#22097 = CARTESIAN_POINT ( 'NONE',  ( 55.81481816583843170, 14.00000000000000178, 14.93194885905434610 ) ) ;
#22098 = CARTESIAN_POINT ( 'NONE',  ( 70.35000000109248219, 11.46158073645647235, 16.46158073645647235 ) ) ;
#22099 = PRESENTATION_LAYER_ASSIGNMENT (  '', '', ( #696 ) ) ;
#22100 = CARTESIAN_POINT ( 'NONE',  ( -72.50000000000000000, 9.999999999999998224, 14.99999999999999645 ) ) ;
#22101 = CARTESIAN_POINT ( 'NONE',  ( 70.60000000109246798, 10.85617417291294551, 17.06698729999999742 ) ) ;
#22102 = EDGE_LOOP ( 'NONE', ( #3291, #11636 ) ) ;
#22103 = CARTESIAN_POINT ( 'NONE',  ( -3.999999999999999112, 0.000000000000000000, 19.12500000273119838 ) ) ;
#22104 = AXIS2_PLACEMENT_3D ( 'NONE', #9208, #11484, #430 ) ;
#22105 = CYLINDRICAL_SURFACE ( 'NONE', #8796, 4.000000000000001776 ) ;
#22106 = AXIS2_PLACEMENT_3D ( 'NONE', #12730, #11161, #23591 ) ;
#22107 = CARTESIAN_POINT ( 'NONE',  ( 54.71643183416158251, 13.97181229448536399, 16.72490539043799629 ) ) ;
#22108 = CARTESIAN_POINT ( 'NONE',  ( 3.689044737729619161, 1.278153343311797085, 2.040000000000004921 ) ) ;
#22109 = CARTESIAN_POINT ( 'NONE',  ( -65.00000000000000000, 9.999999999999998224, 14.99999999999999645 ) ) ;
#22110 = CARTESIAN_POINT ( 'NONE',  ( 4.999999999999999112, 0.4999240074895661690, -8.734705317681621395 ) ) ;
#22111 = B_SPLINE_CURVE_WITH_KNOTS ( 'NONE', 3,
 ( #4383, #18987, #2816, #17215, #2928, #17568, #4742, #9919 ),
 .UNSPECIFIED., .F., .F.,
 ( 4, 2, 2, 4 ),
 ( 2.465131517390770070E-07, 0.001183067374689869946, 0.001774477805458935659, 0.002365888236228001588 ),
 .UNSPECIFIED. ) ;
#22112 = DIRECTION ( 'NONE',  ( -1.224646799147353207E-16, 0.000000000000000000, -1.000000000000000000 ) ) ;
#22113 = VERTEX_POINT ( 'NONE', #23484 ) ;
#22115 = ADVANCED_FACE ( 'NONE', ( #1090 ), #21310, .T. ) ;
#22114 = DIRECTION ( 'NONE',  ( 0.000000000000000000, -0.000000000000000000, -1.000000000000000000 ) ) ;
#22116 = LINE ( 'NONE', #5738, #16666 ) ;
#22117 = CARTESIAN_POINT ( 'NONE',  ( 45.00000000000000000, -2.399706452296352932, 60.00000000000021316 ) ) ;
#22119 = ADVANCED_FACE ( 'NONE', ( #17646 ), #12032, .F. ) ;
#22118 = VECTOR ( 'NONE', #709, 1000.000000000000000 ) ;
#22120 = EDGE_CURVE ( 'NONE', #13999, #13486, #13761, .T. ) ;
#22121 = EDGE_LOOP ( 'NONE', ( #21924, #16492, #3090, #18524 ) ) ;
#22122 = CIRCLE ( 'NONE', #13735, 2.500000000000007550 ) ;
#22123 = DIRECTION ( 'NONE',  ( 0.000000000000000000, 0.8090169943749485615, -0.5877852522924714718 ) ) ;
#22124 = CARTESIAN_POINT ( 'NONE',  ( 4.999999999999999112, 0.000000000000000000, 0.000000000000000000 ) ) ;
#22125 = CARTESIAN_POINT ( 'NONE',  ( -19.99999999999999645, -9.000000000000003553, 10.00000000000008882 ) ) ;
#22126 = CARTESIAN_POINT ( 'NONE',  ( 4.999999999999999112, 6.478011392632890164, 6.807171995660607600 ) ) ;
#22127 = ORIENTED_EDGE ( 'NONE', *, *, #15954, .T. ) ;
#22128 = LINE ( 'NONE', #5391, #22521 ) ;
#22129 = EDGE_LOOP ( 'NONE', ( #16833, #13834, #8830, #16297 ) ) ;
#22130 = PRODUCT_DEFINITION_FORMATION_WITH_SPECIFIED_SOURCE ( 'ANY', '', #13562, .NOT_KNOWN. ) ;
#22131 = CARTESIAN_POINT ( 'NONE',  ( 2.828427124746191179, 2.828427124746190291, 18.75000000273119483 ) ) ;
#22132 = VECTOR ( 'NONE', #1249, 1000.000000000000114 ) ;
#22133 = CARTESIAN_POINT ( 'NONE',  ( 1.971781867644420635E-15, -4.000000000000000000, 14.25000000000001066 ) ) ;
#22134 = DIRECTION ( 'NONE',  ( 0.000000000000000000, -0.5877852522924624790, -0.8090169943749551118 ) ) ;
#22135 = CIRCLE ( 'NONE', #3783, 4.000000000000001776 ) ;
#22136 = DIRECTION ( 'NONE',  ( 1.000000000000000000, -0.000000000000000000, -0.000000000000000000 ) ) ;
#22137 = CARTESIAN_POINT ( 'NONE',  ( 69.65000000109246514, 12.06698730000000097, 14.99999999999999645 ) ) ;
#22138 = CIRCLE ( 'NONE', #7645, 5.000000000000011546 ) ;
#22139 = ORIENTED_EDGE ( 'NONE', *, *, #22978, .T. ) ;
#22140 = AXIS2_PLACEMENT_3D ( 'NONE', #21520, #20078, #3805 ) ;
#22141 = CARTESIAN_POINT ( 'NONE',  ( 1.567478505476134606E-15, 4.618802153517012066, -3.433295621305382905 ) ) ;
#22142 = CARTESIAN_POINT ( 'NONE',  ( 66.40000000218495302, 7.499999999999996447, 14.99999999999999645 ) ) ;
#22143 = CARTESIAN_POINT ( 'NONE',  ( 65.85000000109248219, 7.933012699999995476, 14.99999999999999645 ) ) ;
#22144 = CARTESIAN_POINT ( 'NONE',  ( -1.432654583217639610, -3.458734124999999882, 15.62500000136560629 ) ) ;
#22145 = CARTESIAN_POINT ( 'NONE',  ( 2.500000000000000000, 0.000000000000000000, 0.000000000000000000 ) ) ;
#22146 = AXIS2_PLACEMENT_3D ( 'NONE', #12640, #16207, #1808 ) ;
#22147 = CARTESIAN_POINT ( 'NONE',  ( -3.458734125000000770, 1.432654583217640498, -3.074999998634403209 ) ) ;
#22148 = CARTESIAN_POINT ( 'NONE',  ( 1.656854249492383024, -3.999999999999999112, 4.612500000000001599 ) ) ;
#22149 = CARTESIAN_POINT ( 'NONE',  ( -71.35000000218497007, 8.964466094067278235, 12.49999999999997691 ) ) ;
#22150 = CARTESIAN_POINT ( 'NONE',  ( -1.432654583217638944, 3.458734125000000326, 12.25000000136560452 ) ) ;
#22151 = LINE ( 'NONE', #22272, #17983 ) ;
#22152 = ORIENTED_EDGE ( 'NONE', *, *, #5326, .T. ) ;
#22153 = CARTESIAN_POINT ( 'NONE',  ( -69.90000000109247935, 7.933012699999995476, 14.14382582708705094 ) ) ;
#22154 = EDGE_LOOP ( 'NONE', ( #6271, #4572, #19541, #19865 ) ) ;
#22155 = CARTESIAN_POINT ( 'NONE',  ( 57.09375000000000711, 11.65685424949236193, 10.99999999999998401 ) ) ;
#22156 = CARTESIAN_POINT ( 'NONE',  ( -71.95000000109247651, 11.46158073645647235, 13.53841926354352232 ) ) ;
#22157 = APPLICATION_PROTOCOL_DEFINITION ( 'draft international standard', 'automotive_design', 1998, #12233 ) ;
#22158 = VERTEX_POINT ( 'NONE', #3248 ) ;
#22159 = CARTESIAN_POINT ( 'NONE',  ( 2.828427124746192067, -2.828427124746189847, 17.37500000000001066 ) ) ;
#22160 = VERTEX_POINT ( 'NONE', #16083 ) ;
#22161 = AXIS2_PLACEMENT_3D ( 'NONE', #910, #23064, #15564 ) ;
#22162 = ORIENTED_EDGE ( 'NONE', *, *, #16094, .T. ) ;
#22163 = CARTESIAN_POINT ( 'NONE',  ( 3.458734125000001658, 4.235727675282972223E-16, 18.18750000136560274 ) ) ;
#22164 = CARTESIAN_POINT ( 'NONE',  ( 56.53125000000000711, 11.24264068711929276, 18.00000000000000355 ) ) ;
#22165 = CIRCLE ( 'NONE', #17981, 0.2000000000000005107 ) ;
#22166 = EDGE_CURVE ( 'NONE', #6908, #4668, #18451, .T. ) ;
#22167 = CARTESIAN_POINT ( 'NONE',  ( -71.20000000109246230, 10.85617417291294551, 17.06698729999999742 ) ) ;
#22168 = AXIS2_PLACEMENT_3D ( 'NONE', #5289, #239, #2034 ) ;
#22169 = CARTESIAN_POINT ( 'NONE',  ( 69.75000000109247367, 8.538419263543522320, 16.46158073645647235 ) ) ;
#22170 = CARTESIAN_POINT ( 'NONE',  ( -71.25000000109247367, 12.06698730000000097, 14.99999999999999645 ) ) ;
#22171 = CARTESIAN_POINT ( 'NONE',  ( 1.432654583217641386, 3.458734125000000770, 11.37500000136560452 ) ) ;
#22172 = CARTESIAN_POINT ( 'NONE',  ( -20.00000000000001066, 4.500000000000003553, -49.99999999999999289 ) ) ;
#22173 = CARTESIAN_POINT ( 'NONE',  ( 54.18750000000000711, 9.999999999999989342, 11.99999999999999467 ) ) ;
#22174 = CARTESIAN_POINT ( 'NONE',  ( 1.600000000000004086, 0.000000000000000000, 0.000000000000000000 ) ) ;
#22175 = CARTESIAN_POINT ( 'NONE',  ( -3.458734125000000770, 1.432654583217640498, 5.925000001365596347 ) ) ;
#22176 = CARTESIAN_POINT ( 'NONE',  ( 1.411581201560190495E-15, 4.862606272033091592, -3.745885042887436622 ) ) ;
#22177 = CARTESIAN_POINT ( 'NONE',  ( -2.828427124746188515, -2.828427124746190735, 16.25000000273119838 ) ) ;
#22178 = CARTESIAN_POINT ( 'NONE',  ( -0.7060087303327398089, -11.25000000000000355, 5.000000000000079936 ) ) ;
#22179 = CIRCLE ( 'NONE', #1535, 2.100000000000000089 ) ;
#22180 = VERTEX_POINT ( 'NONE', #10233 ) ;
#22181 = LINE ( 'NONE', #14571, #4854 ) ;
#22182 = CARTESIAN_POINT ( 'NONE',  ( 21.28513981966725765, -11.25000000000000355, 5.000000000000079936 ) ) ;
#22183 = ORIENTED_EDGE ( 'NONE', *, *, #15076, .F. ) ;
#22184 = CARTESIAN_POINT ( 'NONE',  ( 55.31250000000000711, 13.00000000000000000, 14.99999999999998757 ) ) ;
#22185 = VECTOR ( 'NONE', #10572, 1000.000000000000000 ) ;
#22186 = CARTESIAN_POINT ( 'NONE',  ( 6.353591512924457348E-16, -3.458734125000000326, 3.987500001365595015 ) ) ;
#22187 = CARTESIAN_POINT ( 'NONE',  ( 0.000000000000000000, 0.000000000000000000, 3.059999999999998277 ) ) ;
#22188 = VERTEX_POINT ( 'NONE', #13939 ) ;
#22189 = CARTESIAN_POINT ( 'NONE',  ( -3.999999999999998224, -1.656854249492383246, 13.06250000000001066 ) ) ;
#22190 = DIRECTION ( 'NONE',  ( 0.000000000000000000, 1.224646799147333486E-16, 1.000000000000000000 ) ) ;
#22191 = CARTESIAN_POINT ( 'NONE',  ( -2.449293598294706907E-16, 4.000000000000000000, -2.824999997268812457 ) ) ;
#22192 = ORIENTED_EDGE ( 'NONE', *, *, #6200, .F. ) ;
#22193 = EDGE_CURVE ( 'NONE', #19809, #13130, #12049, .T. ) ;
#22194 = CYLINDRICAL_SURFACE ( 'NONE', #22840, 2.500000000000002220 ) ;
#22195 = EDGE_CURVE ( 'NONE', #8728, #12130, #22537, .T. ) ;
#22196 = CARTESIAN_POINT ( 'NONE',  ( 1.432654583217640276, 3.458734125000000770, 0.6750000013655963471 ) ) ;
#22197 = AXIS2_PLACEMENT_3D ( 'NONE', #12475, #21281, #8878 ) ;
#22198 = CARTESIAN_POINT ( 'NONE',  ( 67.09999999999999432, 7.499999999999996447, 14.99999999999999645 ) ) ;
#22199 = EDGE_CURVE ( 'NONE', #22527, #18533, #21435, .T. ) ;
#22200 = PLANE ( 'NONE',  #513 ) ;
#22201 = CARTESIAN_POINT ( 'NONE',  ( -67.14999999999999147, 7.499999999999996447, 13.96446609406725514 ) ) ;
#22202 = CARTESIAN_POINT ( 'NONE',  ( 58.62731816583843170, 12.16943976678978601, 17.07320092032949432 ) ) ;
#22203 = CARTESIAN_POINT ( 'NONE',  ( 1.432654583217642275, -3.458734124999999437, 0.05000000136559582670 ) ) ;
#22204 = CARTESIAN_POINT ( 'NONE',  ( 3.458734125000001658, 1.432654583217640498, 13.25000000136560452 ) ) ;
#22205 = CARTESIAN_POINT ( 'NONE',  ( 2.500000000000000000, -1.768423874527825568, -1.020999999999998575 ) ) ;
#22206 = CARTESIAN_POINT ( 'NONE',  ( -70.80000000109245661, 7.933012699999995476, 15.85617417291294196 ) ) ;
#22207 = CARTESIAN_POINT ( 'NONE',  ( 25.86052135323381407, -9.000000000000001776, 5.000000000000079936 ) ) ;
#22208 = ORIENTED_EDGE ( 'NONE', *, *, #871, .T. ) ;
#22209 = LINE ( 'NONE', #11356, #19121 ) ;
#22210 = DIRECTION ( 'NONE',  ( 0.000000000000000000, 0.000000000000000000, 1.000000000000000000 ) ) ;
#22211 = CARTESIAN_POINT ( 'NONE',  ( 4.999999999999999112, 8.734705317681626724, 0.4999240074894746311 ) ) ;
#22212 = VECTOR ( 'NONE', #14737, 1000.000000000000000 ) ;
#22213 = VERTEX_POINT ( 'NONE', #17866 ) ;
#22214 = ORIENTED_EDGE ( 'NONE', *, *, #5730, .F. ) ;
#22215 = CARTESIAN_POINT ( 'NONE',  ( 2.500000000000000000, 2.357898499370431722, -2.818925648462311528E-15 ) ) ;
#22216 =( BOUNDED_CURVE ( )  B_SPLINE_CURVE ( 2, ( #11908, #2761, #10104, #22885, #21077, #10222, #12134, #2994, #19876 ),
 .UNSPECIFIED., .F., .F. ) 
 B_SPLINE_CURVE_WITH_KNOTS ( ( 3, 2, 2, 2, 3 ),
 ( 0.5999999999999999778, 0.6125000000000000444, 0.6250000000000000000, 0.6374999999999999556, 0.6500000000000000222 ),
 .UNSPECIFIED. ) 
 CURVE ( )  GEOMETRIC_REPRESENTATION_ITEM ( )  RATIONAL_B_SPLINE_CURVE ( ( 1.000000000000000000, 0.9238795325112867385, 1.000000000000000000, 0.9238795325112867385, 1.000000000000000000, 0.9238795325112867385, 1.000000000000000000, 0.9238795325112867385, 1.000000000000000000 ) ) 
 REPRESENTATION_ITEM ( '' )  );
#22217 = CARTESIAN_POINT ( 'NONE',  ( 53.15625000000000711, 6.000000000000004441, 16.65685424949239390 ) ) ;
#22218 = EDGE_LOOP ( 'NONE', ( #14486, #15056, #13010, #20209 ) ) ;
#22219 = LINE ( 'NONE', #14607, #20196 ) ;
#22220 = ORIENTED_EDGE ( 'NONE', *, *, #16857, .T. ) ;
#22221 = CARTESIAN_POINT ( 'NONE',  ( 56.47106816583845301, 5.971812294485345340, 13.41119689145326710 ) ) ;
#22222 = ADVANCED_FACE ( 'NONE', ( #3773 ), #17924, .T. ) ;
#22223 = ADVANCED_FACE ( 'NONE', ( #14237 ), #16808, .T. ) ;
#22224 = CARTESIAN_POINT ( 'NONE',  ( 70.90000000109246514, 10.85617417291294551, 12.93301269999999370 ) ) ;
#22225 = B_SPLINE_CURVE_WITH_KNOTS ( 'NONE', 3,
 ( #19225, #2812, #4140, #22811, #13507, #17208 ),
 .UNSPECIFIED., .F., .F.,
 ( 4, 2, 4 ),
 ( 0.003358874760055551890, 0.004541967308452098118, 0.005725059856848645212 ),
 .UNSPECIFIED. ) ;
#22226 = DIRECTION ( 'NONE',  ( 0.000000000000000000, 0.000000000000000000, 1.000000000000000000 ) ) ;
#22227 = DIRECTION ( 'NONE',  ( 0.000000000000000000, 0.000000000000000000, 1.000000000000000000 ) ) ;
#22228 = EDGE_CURVE ( 'NONE', #14446, #16796, #7398, .T. ) ;
#22229 = ORIENTED_EDGE ( 'NONE', *, *, #16249, .F. ) ;
#22230 = CARTESIAN_POINT ( 'NONE',  ( -3.999999999999999112, 0.000000000000000000, 15.12500000273119660 ) ) ;
#22231 = EDGE_CURVE ( 'NONE', #8738, #3905, #9078, .T. ) ;
#22232 = DIRECTION ( 'NONE',  ( -0.000000000000000000, -1.000000000000000000, -0.000000000000000000 ) ) ;
#22233 = CARTESIAN_POINT ( 'NONE',  ( 53.02893183416157541, 11.58880310854676132, 19.02818770551463956 ) ) ;
#22234 = CARTESIAN_POINT ( 'NONE',  ( -14.98942794071655271, -8.974600000000002353, 5.000000000000079936 ) ) ;
#22235 = CARTESIAN_POINT ( 'NONE',  ( 4.999999999999999112, 5.538577986808900455, 6.772677083992405755 ) ) ;
#22236 = CARTESIAN_POINT ( 'NONE',  ( 7.000000000000000000, 0.000000000000000000, 1.734723475976807094E-15 ) ) ;
#22237 = CARTESIAN_POINT ( 'NONE',  ( 0.000000000000000000, 0.000000000000000000, 0.000000000000000000 ) ) ;
#22238 = CARTESIAN_POINT ( 'NONE',  ( -20.00000000000001066, 9.999999999999964473, -49.99999999999999289 ) ) ;
#22239 = VERTEX_POINT ( 'NONE', #12797 ) ;
#22240 = CARTESIAN_POINT ( 'NONE',  ( 45.00000000000000000, -9.796556200126357083, 5.000000000000079936 ) ) ;
#22241 = CARTESIAN_POINT ( 'NONE',  ( 53.43750000000000711, 10.00000000000000711, 17.99999999999999645 ) ) ;
#22242 = CARTESIAN_POINT ( 'NONE',  ( 0.000000000000000000, 0.000000000000000000, 0.000000000000000000 ) ) ;
#22243 = EDGE_LOOP ( 'NONE', ( #18866, #10080, #21557, #3233 ) ) ;
#22244 = CARTESIAN_POINT ( 'NONE',  ( 69.05000000218494449, 11.03553390593276262, 12.50000000000001776 ) ) ;
#22245 = LINE ( 'NONE', #11156, #4145 ) ;
#22246 = CARTESIAN_POINT ( 'NONE',  ( 1.734723475976807094E-15, 4.618802153517012954, -0.4999999999999995559 ) ) ;
#22247 = DIRECTION ( 'NONE',  ( -1.224646799147353207E-16, 0.000000000000000000, -1.000000000000000000 ) ) ;
#22248 = ORIENTED_EDGE ( 'NONE', *, *, #15533, .F. ) ;
#22249 = DIRECTION ( 'NONE',  ( -0.000000000000000000, 1.000000000000000000, -0.000000000000000000 ) ) ;
#22250 = ORIENTED_EDGE ( 'NONE', *, *, #23298, .T. ) ;
#22251 = CARTESIAN_POINT ( 'NONE',  ( -20.00005080000000035, 0.000000000000000000, -1.000000000000000000 ) ) ;
#22252 = ADVANCED_FACE ( 'NONE', ( #1853 ), #3431, .F. ) ;
#22253 = CARTESIAN_POINT ( 'NONE',  ( 4.000000000000000888, 1.656854249492381248, 14.56250000000001066 ) ) ;
#22254 = DIRECTION ( 'NONE',  ( -1.000000000000000000, -0.000000000000000000, -0.000000000000000000 ) ) ;
#22255 = CARTESIAN_POINT ( 'NONE',  ( 4.999999999999999112, 7.593217523260696211, -7.958834565716683684 ) ) ;
#22256 = EDGE_CURVE ( 'NONE', #22912, #15687, #19847, .T. ) ;
#22257 = FILL_AREA_STYLE ('',( #7912 ) ) ;
#22258 = CARTESIAN_POINT ( 'NONE',  ( 70.95000000109247651, 8.538419263543524096, 13.53841926354352054 ) ) ;
#22259 = ORIENTED_EDGE ( 'NONE', *, *, #9725, .F. ) ;
#22260 = EDGE_CURVE ( 'NONE', #8348, #23470, #22916, .T. ) ;
#22261 = CARTESIAN_POINT ( 'NONE',  ( -3.333333333333335258, 2.694301256218251783, -3.300726591567079815 ) ) ;
#22262 = VECTOR ( 'NONE', #17592, 1000.000000000000000 ) ;
#22263 = DIRECTION ( 'NONE',  ( -1.000000000000000000, 0.000000000000000000, -0.000000000000000000 ) ) ;
#22264 = CIRCLE ( 'NONE', #20345, 4.000000000000002665 ) ;
#22265 = CARTESIAN_POINT ( 'NONE',  ( 71.90000000109246514, 10.85617417291294551, 12.93301269999999370 ) ) ;
#22266 = CARTESIAN_POINT ( 'NONE',  ( 2.445694354108821411, 2.445694354108820523, 17.06250000136560629 ) ) ;
#22267 = CARTESIAN_POINT ( 'NONE',  ( 0.000000000000000000, -9.241976615262146311, 2.300561732649528679 ) ) ;
#22268 = CARTESIAN_POINT ( 'NONE',  ( 0.000000000000000000, -1.178949249685214307, 2.042000000000001592 ) ) ;
#22269 = CARTESIAN_POINT ( 'NONE',  ( -1.656854249492380804, 4.000000000000000000, 1.112500000000000711 ) ) ;
#22270 = CARTESIAN_POINT ( 'NONE',  ( 1.656854249492383024, -3.999999999999999112, -3.262499997268812901 ) ) ;
#22271 = CARTESIAN_POINT ( 'NONE',  ( 3.458734125000001214, 1.432654583217640498, 15.00000000136560629 ) ) ;
#22272 = CARTESIAN_POINT ( 'NONE',  ( 4.999999999999999112, -0.4999240074895051067, 8.734705317681624948 ) ) ;
#22273 = EDGE_LOOP ( 'NONE', ( #18395, #6461, #23202, #811 ) ) ;
#22274 = CARTESIAN_POINT ( 'NONE',  ( -69.10000000109248219, 7.933012699999995476, 14.14382582708705094 ) ) ;
#22275 = VERTEX_POINT ( 'NONE', #20050 ) ;
#22276 = CARTESIAN_POINT ( 'NONE',  ( 52.18518183416157541, 10.06805114094561659, 10.99999999999999645 ) ) ;
#22277 = CARTESIAN_POINT ( 'NONE',  ( -71.35000000109246798, 11.46158073645647235, 16.46158073645647235 ) ) ;
#22278 = VERTEX_POINT ( 'NONE', #1623 ) ;
#22279 = CARTESIAN_POINT ( 'NONE',  ( 2.828427124746189847, 2.828427124746190291, 1.050000002731187321 ) ) ;
#22280 = ORIENTED_EDGE ( 'NONE', *, *, #15412, .T. ) ;
#22281 = VERTEX_POINT ( 'NONE', #23310 ) ;
#22282 = CARTESIAN_POINT ( 'NONE',  ( 1.872352939448454495E-15, -3.458734125000000770, 16.93750000136560629 ) ) ;
#22283 = CARTESIAN_POINT ( 'NONE',  ( 54.18750000000000711, 9.999999999999989342, 11.99999999999999467 ) ) ;
#22284 = CARTESIAN_POINT ( 'NONE',  ( -67.70000000109246230, 10.85617417291294551, 12.93301269999999370 ) ) ;
#22285 = AXIS2_PLACEMENT_3D ( 'NONE', #7249, #17897, #8934 ) ;
#22286 = CARTESIAN_POINT ( 'NONE',  ( 69.10000000109248219, 7.933012699999995476, 14.14382582708705094 ) ) ;
#22287 = ADVANCED_FACE ( 'NONE', ( #23546 ), #7282, .T. ) ;
#22288 = MANIFOLD_SOLID_BREP ( 'Fillet1', #20779 ) ;
#22289 = CARTESIAN_POINT ( 'NONE',  ( -67.70000000109246230, 7.933012699999995476, 14.14382582708705094 ) ) ;
#22290 = CARTESIAN_POINT ( 'NONE',  ( 1.025207404391860050E-15, 3.458734125000000770, 11.43750000136560452 ) ) ;
#22291 = DIRECTION ( 'NONE',  ( 0.5000000000000004441, -0.8660254037844383745, 0.000000000000000000 ) ) ;
#22292 = CARTESIAN_POINT ( 'NONE',  ( 55.46643183416158962, 7.028187705514638672, 13.68930817193508531 ) ) ;
#22293 = DIRECTION ( 'NONE',  ( 1.000000000000000000, 0.000000000000000000, 0.000000000000000000 ) ) ;
#22294 = CARTESIAN_POINT ( 'NONE',  ( 52.87500000000000711, 7.878679656440349177, 12.87867965644035984 ) ) ;
#22295 = CARTESIAN_POINT ( 'NONE',  ( 2.445694354108821411, 2.445694354108820523, 12.06250000136560629 ) ) ;
#22296 = CARTESIAN_POINT ( 'NONE',  ( 1.656854249492381470, 4.000000000000000000, 16.81250000273119838 ) ) ;
#22297 = CARTESIAN_POINT ( 'NONE',  ( 45.00000000000000000, 2.399706452296377801, 55.00000000000021316 ) ) ;
#22298 = AXIS2_PLACEMENT_3D ( 'NONE', #999, #11471, #18747 ) ;
#22299 = ORIENTED_EDGE ( 'NONE', *, *, #8339, .F. ) ;
#22300 = CARTESIAN_POINT ( 'NONE',  ( -1.600000000000004086, 8.247996192257451316E-16, 6.735000000000022524 ) ) ;
#22301 = ORIENTED_EDGE ( 'NONE', *, *, #5298, .T. ) ;
#22302 = CARTESIAN_POINT ( 'NONE',  ( 58.65393183416157541, 6.971812294485357775, 16.17458954617365663 ) ) ;
#22303 =( NAMED_UNIT ( * ) SI_UNIT ( $, .STERADIAN. ) SOLID_ANGLE_UNIT ( ) );
#22304 = CARTESIAN_POINT ( 'NONE',  ( 2.828427124746189847, 2.828427124746190291, -1.949999997268811791 ) ) ;
#22305 = AXIS2_PLACEMENT_3D ( 'NONE', #13916, #6955, #9001 ) ;
#22306 = DIRECTION ( 'NONE',  ( 7.200064461366508930E-32, 1.000000000000000000, 5.754033390038003495E-16 ) ) ;
#22307 = ORIENTED_EDGE ( 'NONE', *, *, #14674, .F. ) ;
#22308 = CARTESIAN_POINT ( 'NONE',  ( 1.656854249492381470, 4.000000000000000000, 11.68750000000001066 ) ) ;
#22309 = CARTESIAN_POINT ( 'NONE',  ( -2.338817011410299154E-16, 3.819578041666666923, -3.054166666211466374 ) ) ;
#22310 = CARTESIAN_POINT ( 'NONE',  ( 2.828427124746191179, 2.828427124746190291, 14.62500000000000888 ) ) ;
#22311 = ORIENTED_EDGE ( 'NONE', *, *, #2307, .T. ) ;
#22312 = PRODUCT_DEFINITION_SHAPE ( 'NONE', 'NONE',  #23715 ) ;
#22313 = CARTESIAN_POINT ( 'NONE',  ( -70.35000000218492744, 7.499999999999995559, 16.03553390593273420 ) ) ;
#22314 = CARTESIAN_POINT ( 'NONE',  ( 1.432654583217642053, -3.458734124999999882, -0.6999999986344028757 ) ) ;
#22315 = B_SPLINE_CURVE_WITH_KNOTS ( 'NONE', 1,
 ( #15040, #20503 ),
 .UNSPECIFIED., .F., .F.,
 ( 2, 2 ),
 ( 0.000000000000000000, 1.000000000000000000 ),
 .UNSPECIFIED. ) ;
#22316 = CARTESIAN_POINT ( 'NONE',  ( 67.34999999999999432, 11.03553390593273598, 12.49999999999999289 ) ) ;
#22317 = CARTESIAN_POINT ( 'NONE',  ( 4.000000000000000888, 4.898587196589412829E-16, 21.31370849898476649 ) ) ;
#22318 = CARTESIAN_POINT ( 'NONE',  ( 0.000000000000000000, 0.000000000000000000, 1.734723475976807094E-15 ) ) ;
#22319 = CARTESIAN_POINT ( 'NONE',  ( 50.75231816583844591, 7.219692298483957771, 17.87654654797633924 ) ) ;
#22320 = CARTESIAN_POINT ( 'NONE',  ( 3.458734125000000770, 4.235727675282972223E-16, 5.487500001365596347 ) ) ;
#22321 = CARTESIAN_POINT ( 'NONE',  ( -3.458734124999998993, -1.432654583217642497, 16.75000000136560629 ) ) ;
#22322 = FACE_OUTER_BOUND ( 'NONE', #6125, .T. ) ;
#22323 = MANIFOLD_SOLID_BREP ( 'Cavity1', #17741 ) ;
#22324 = CARTESIAN_POINT ( 'NONE',  ( -71.10000000109246798, 10.85617417291294551, 12.93301269999999192 ) ) ;
#22325 = EDGE_CURVE ( 'NONE', #18556, #12818, #15067, .T. ) ;
#22326 = CARTESIAN_POINT ( 'NONE',  ( -69.99999999999998579, 11.76776695296636888, 16.76776695296636532 ) ) ;
#22327 = ORIENTED_EDGE ( 'NONE', *, *, #8238, .F. ) ;
#22328 = CARTESIAN_POINT ( 'NONE',  ( 2.828427124746192067, -2.828427124746189847, 14.37500000000001066 ) ) ;
#22329 = CARTESIAN_POINT ( 'NONE',  ( -65.65000000109247935, 9.999999999999998224, 17.06698730000000097 ) ) ;
#22330 = CARTESIAN_POINT ( 'NONE',  ( -72.00000000109248788, 10.85617417291294551, 17.06698729999999742 ) ) ;
#22331 = ORIENTED_EDGE ( 'NONE', *, *, #21483, .F. ) ;
#22332 = VERTEX_POINT ( 'NONE', #7154 ) ;
#22333 = DIRECTION ( 'NONE',  ( -1.224646799147353207E-16, 0.000000000000000000, -1.000000000000000000 ) ) ;
#22334 = EDGE_CURVE ( 'NONE', #549, #2702, #13387, .T. ) ;
#22335 = DIRECTION ( 'NONE',  ( -0.000000000000000000, -1.000000000000000000, -0.000000000000000000 ) ) ;
#22336 = ORIENTED_EDGE ( 'NONE', *, *, #10831, .T. ) ;
#22337 = CARTESIAN_POINT ( 'NONE',  ( -20.00005080000000035, 0.000000000000000000, -6.000000000000000888 ) ) ;
#22338 = VERTEX_POINT ( 'NONE', #295 ) ;
#22339 = CARTESIAN_POINT ( 'NONE',  ( 54.78356816583844591, 8.275094609561968184, 11.02818770551464667 ) ) ;
#22340 = CARTESIAN_POINT ( 'NONE',  ( 66.20000000218495018, 9.999999999999998224, 17.49999999999999645 ) ) ;
#22341 = AXIS2_PLACEMENT_3D ( 'NONE', #11572, #15398, #22900 ) ;
#22342 = CARTESIAN_POINT ( 'NONE',  ( 66.19999999999998863, 8.232233047033627571, 16.76776695296636532 ) ) ;
#22343 = CARTESIAN_POINT ( 'NONE',  ( 71.15000000109246514, 11.46158073645647235, 13.53841926354352232 ) ) ;
#22344 = VECTOR ( 'NONE', #14503, 1000.000000000000000 ) ;
#22345 = ORIENTED_EDGE ( 'NONE', *, *, #4663, .T. ) ;
#22346 = CARTESIAN_POINT ( 'NONE',  ( -3.999999999999999112, 0.000000000000000000, 13.12500000273119660 ) ) ;
#22347 = DIRECTION ( 'NONE',  ( 0.000000000000000000, 0.000000000000000000, -1.000000000000000000 ) ) ;
#22348 = CARTESIAN_POINT ( 'NONE',  ( 53.59143183416158962, 11.72490539043799984, 11.02818770551463246 ) ) ;
#22349 = PLANE ( 'NONE',  #12314 ) ;
#22350 = CARTESIAN_POINT ( 'NONE',  ( 0.000000000000000000, 4.472189673936902921, -8.264486777890061475 ) ) ;
#22351 = CYLINDRICAL_SURFACE ( 'NONE', #3263, 12.00000000000000000 ) ;
#22352 = ADVANCED_FACE ( 'NONE', ( #20407 ), #11596, .F. ) ;
#22353 = CARTESIAN_POINT ( 'NONE',  ( -1.656854249492381248, -3.999999999999999112, 0.4875000000000020983 ) ) ;
#22354 = DIRECTION ( 'NONE',  ( 0.000000000000000000, 0.000000000000000000, -1.000000000000000000 ) ) ;
#22355 = ORIENTED_EDGE ( 'NONE', *, *, #8478, .F. ) ;
#22356 = EDGE_CURVE ( 'NONE', #17055, #8937, #11109, .T. ) ;
#22357 = CARTESIAN_POINT ( 'NONE',  ( 51.65625000000000711, 7.000000000000002665, 16.24264068711929099 ) ) ;
#22358 = DIRECTION ( 'NONE',  ( 1.000000000000000000, 0.000000000000000000, 0.000000000000000000 ) ) ;
#22359 = ORIENTED_EDGE ( 'NONE', *, *, #15818, .F. ) ;
#22360 = FACE_BOUND ( 'NONE', #10220, .T. ) ;
#22361 = DIRECTION ( 'NONE',  ( -1.000000000000000000, 0.000000000000000000, 0.000000000000000000 ) ) ;
#22362 = FACE_OUTER_BOUND ( 'NONE', #16993, .T. ) ;
#22363 = AXIS2_PLACEMENT_3D ( 'NONE', #8946, #10861, #20032 ) ;
#22364 = AXIS2_PLACEMENT_3D ( 'NONE', #20051, #7752, #16718 ) ;
#22365 = ADVANCED_FACE ( 'NONE', ( #22322 ), #17078, .F. ) ;
#22366 = DIRECTION ( 'NONE',  ( 7.087422195345011518E-32, 1.000000000000000000, -0.000000000000000000 ) ) ;
#22367 = ORIENTED_EDGE ( 'NONE', *, *, #7503, .F. ) ;
#22368 = FACE_BOUND ( 'NONE', #17360, .T. ) ;
#22369 = ORIENTED_EDGE ( 'NONE', *, *, #23114, .F. ) ;
#22370 = CARTESIAN_POINT ( 'NONE',  ( 4.000000000000000000, 4.898587196589412829E-16, 1.800000000000001155 ) ) ;
#22371 = CARTESIAN_POINT ( 'NONE',  ( 1.656854249492381470, 4.000000000000000000, 13.68750000000001066 ) ) ;
#22372 = FACE_OUTER_BOUND ( 'NONE', #15606, .T. ) ;
#22373 = B_SPLINE_CURVE_WITH_KNOTS ( 'NONE', 3,
 ( #3639, #22309, #5679, #13014 ),
 .UNSPECIFIED., .F., .F.,
 ( 4, 4 ),
 ( 0.000000000000000000, 1.000000000000000000 ),
 .UNSPECIFIED. ) ;
#22374 = CARTESIAN_POINT ( 'NONE',  ( 118.3095189484530181, 10.00000000000001599, 17.50000000000003908 ) ) ;
#22375 = CARTESIAN_POINT ( 'NONE',  ( -2.828427124746189403, 2.828427124746190291, 18.00000000273119483 ) ) ;
#22376 = CARTESIAN_POINT ( 'NONE',  ( 71.85000000109246798, 9.999999999999998224, 12.93301269999999192 ) ) ;
#22377 = ORIENTED_EDGE ( 'NONE', *, *, #22832, .F. ) ;
#22378 = CIRCLE ( 'NONE', #23151, 5.384454397937118664 ) ;
#22379 = LINE ( 'NONE', #3949, #9533 ) ;
#22380 = ADVANCED_FACE ( 'NONE', ( #15183 ), #22442, .T. ) ;
#22381 = CIRCLE ( 'NONE', #15913, 9.000000000000021316 ) ;
#22382 = CARTESIAN_POINT ( 'NONE',  ( 34.99999999999999289, 4.500000000000001776, -50.00000000000000000 ) ) ;
#22383 = CARTESIAN_POINT ( 'NONE',  ( 66.20000000109247651, 12.06698730000000275, 14.14382582708705094 ) ) ;
#22384 = CARTESIAN_POINT ( 'NONE',  ( -2.445694354108819191, 2.445694354108820523, 13.31250000136560452 ) ) ;
#22385 = CARTESIAN_POINT ( 'NONE',  ( 4.999999999999999112, 0.000000000000000000, 0.000000000000000000 ) ) ;
#22386 = CARTESIAN_POINT ( 'NONE',  ( 3.458734125000000770, 1.432654583217640498, -1.449999998634403653 ) ) ;
#22387 = CARTESIAN_POINT ( 'NONE',  ( -2.449293598294706907E-16, 4.000000000000000000, 2.050000000000001599 ) ) ;
#22388 = EDGE_CURVE ( 'NONE', #4037, #21869, #14493, .T. ) ;
#22389 = CARTESIAN_POINT ( 'NONE',  ( 8.718769219667262149, -11.25000000000000355, 5.000000000000079936 ) ) ;
#22390 = CARTESIAN_POINT ( 'NONE',  ( 3.458734125000002102, -1.432654583217639610, 13.87500000136560452 ) ) ;
#22391 = CARTESIAN_POINT ( 'NONE',  ( -67.30000000218494449, 8.232233047033629347, 13.23223304703362402 ) ) ;
#22392 = CIRCLE ( 'NONE', #2111, 5.000000000000000888 ) ;
#22393 = VECTOR ( 'NONE', #23098, 1000.000000000000114 ) ;
#22394 = VERTEX_POINT ( 'NONE', #15306 ) ;
#22395 = CARTESIAN_POINT ( 'NONE',  ( -66.10000000109248219, 10.85617417291294551, 12.93301269999999192 ) ) ;
#22396 = ORIENTED_EDGE ( 'NONE', *, *, #9661, .F. ) ;
#22397 = CARTESIAN_POINT ( 'NONE',  ( 56.15625000000002132, 6.000000000000004441, 16.65685424949239390 ) ) ;
#22398 = CARTESIAN_POINT ( 'NONE',  ( -70.70000000109247651, 9.143825827087049163, 17.06698729999999742 ) ) ;
#22399 = APPLICATION_PROTOCOL_DEFINITION ( 'draft international standard', 'automotive_design', 1998, #11642 ) ;
#22400 = EDGE_CURVE ( 'NONE', #17853, #7410, #7512, .T. ) ;
#22401 = ORIENTED_EDGE ( 'NONE', *, *, #20465, .F. ) ;
#22402 = CARTESIAN_POINT ( 'NONE',  ( 4.000000000000000000, 4.898587196589412829E-16, -2.074999997268812013 ) ) ;
#22403 = EDGE_LOOP ( 'NONE', ( #2618, #16644, #16653, #12430 ) ) ;
#22404 = ADVANCED_FACE ( 'NONE', ( #22579 ), #14954, .F. ) ;
#22405 = EDGE_LOOP ( 'NONE', ( #1579, #22561, #8760, #14624 ) ) ;
#22406 = CARTESIAN_POINT ( 'NONE',  ( -3.458734124999999437, 1.432654583217640498, 16.62500000136560629 ) ) ;
#22407 = CARTESIAN_POINT ( 'NONE',  ( 55.03125000000000000, 11.24264068711929276, 18.00000000000000355 ) ) ;
#22408 = CARTESIAN_POINT ( 'NONE',  ( -67.30000000109247082, 9.143825827087049163, 17.06698729999999742 ) ) ;
#22409 = CARTESIAN_POINT ( 'NONE',  ( 70.05000000109247082, 9.999999999999998224, 12.93301269999999192 ) ) ;
#22410 = CARTESIAN_POINT ( 'NONE',  ( -66.50000000109245946, 12.06698730000000275, 15.85617417291294196 ) ) ;
#22411 = DIRECTION ( 'NONE',  ( 1.000000000000000000, 0.000000000000000000, 0.000000000000000000 ) ) ;
#22412 = CARTESIAN_POINT ( 'NONE',  ( 55.74768183416157541, 7.830560233210222876, 17.07320092032950498 ) ) ;
#22413 = DIRECTION ( 'NONE',  ( 0.000000000000000000, 0.000000000000000000, -1.000000000000000000 ) ) ;
#22414 = CARTESIAN_POINT ( 'NONE',  ( 1.432654583217642275, -3.458734124999999882, 5.300000001365596347 ) ) ;
#22415 = CARTESIAN_POINT ( 'NONE',  ( -2.445694354108819191, 2.445694354108820523, 11.31250000136560452 ) ) ;
#22416 = CARTESIAN_POINT ( 'NONE',  ( -3.999999999999998224, -1.656854249492383246, 14.18750000273119483 ) ) ;
#22417 = DIRECTION ( 'NONE',  ( 1.000000000000000000, 0.000000000000000000, 0.000000000000000000 ) ) ;
#22418 = VERTEX_POINT ( 'NONE', #22205 ) ;
#22419 = CARTESIAN_POINT ( 'NONE',  ( 45.00000000000000000, 2.399706452296377801, 55.00000000000021316 ) ) ;
#22420 = EDGE_LOOP ( 'NONE', ( #10969, #12914, #17733, #23261 ) ) ;
#22421 = CARTESIAN_POINT ( 'NONE',  ( 55.37268183416157541, 7.926799079670491466, 12.83056023321021755 ) ) ;
#22422 = CARTESIAN_POINT ( 'NONE',  ( -1.432654583217640276, 3.458734125000000326, 2.550000001365598123 ) ) ;
#22423 = EDGE_CURVE ( 'NONE', #433, #1904, #19497, .T. ) ;
#22424 = LINE ( 'NONE', #20633, #12866 ) ;
#22425 = ORIENTED_EDGE ( 'NONE', *, *, #16551, .T. ) ;
#22426 = CARTESIAN_POINT ( 'NONE',  ( 2.828427124746191179, 2.828427124746190291, 13.62500000000001066 ) ) ;
#22427 = EDGE_CURVE ( 'NONE', #9951, #7519, #1301, .T. ) ;
#22428 = CARTESIAN_POINT ( 'NONE',  ( 72.50000000000000000, 9.999999999999998224, 12.49999999999999289 ) ) ;
#22429 = DIRECTION ( 'NONE',  ( 1.224646799147353207E-16, -0.000000000000000000, 1.000000000000000000 ) ) ;
#22430 = EDGE_LOOP ( 'NONE', ( #19999, #14506, #17793, #9592 ) ) ;
#22431 = CIRCLE ( 'NONE', #21674, 5.479999999999998650 ) ;
#22432 = CARTESIAN_POINT ( 'NONE',  ( -70.45000000218493597, 7.499999999999995559, 13.96446609406725692 ) ) ;
#22433 = CARTESIAN_POINT ( 'NONE',  ( -1.432654583217640498, 3.458734125000000770, -2.199999998634404097 ) ) ;
#22434 = CARTESIAN_POINT ( 'NONE',  ( -55.00000000000000000, -15.00000000000000000, 10.00000000000001599 ) ) ;
#22435 = CARTESIAN_POINT ( 'NONE',  ( 68.05000000000002558, 8.964466094067258695, 12.49999999999999289 ) ) ;
#22436 = CARTESIAN_POINT ( 'NONE',  ( -71.04999999999999716, 7.499999999999996447, 16.03553390593273775 ) ) ;
#22437 = CONICAL_SURFACE ( 'NONE', #5237, 4.000000000000000000, 0.9599310885968780349 ) ;
#22438 = DIRECTION ( 'NONE',  ( -1.000000000000000000, 0.000000000000000000, 0.000000000000000000 ) ) ;
#22439 = CARTESIAN_POINT ( 'NONE',  ( 55.06481816583844591, 6.999999999999998224, 15.06805114094563436 ) ) ;
#22440 = CARTESIAN_POINT ( 'NONE',  ( -3.458734125000000770, 1.432654583217640498, 3.925000001365594127 ) ) ;
#22441 = CARTESIAN_POINT ( 'NONE',  ( 2.445694354108821411, 2.445694354108820523, 15.31250000136560452 ) ) ;
#22442 = PLANE ( 'NONE',  #11875 ) ;
#22443 = MANIFOLD_SOLID_BREP ( 'EndChamfer', #14314 ) ;
#22444 = CARTESIAN_POINT ( 'NONE',  ( -70.40000000109247935, 12.06698729999999919, 14.14382582708705094 ) ) ;
#22445 = CARTESIAN_POINT ( 'NONE',  ( -70.09999999999999432, 9.999999999999998224, 17.49999999999999645 ) ) ;
#22446 = ORIENTED_EDGE ( 'NONE', *, *, #15053, .F. ) ;
#22447 = DIRECTION ( 'NONE',  ( 0.000000000000000000, 0.000000000000000000, 1.000000000000000000 ) ) ;
#22448 = CARTESIAN_POINT ( 'NONE',  ( 1.656854249492383024, -3.999999999999999112, 2.737500002731188431 ) ) ;
#22449 = CARTESIAN_POINT ( 'NONE',  ( -70.45000000109247651, 9.999999999999998224, 17.06698730000000097 ) ) ;
#22450 = ORIENTED_EDGE ( 'NONE', *, *, #19599, .T. ) ;
#22451 = ORIENTED_EDGE ( 'NONE', *, *, #2367, .F. ) ;
#22452 = VECTOR ( 'NONE', #13848, 1000.000000000000000 ) ;
#22453 = CARTESIAN_POINT ( 'NONE',  ( -27.50000000000000711, 1.500000000000003109, -33.66025403784446723 ) ) ;
#22454 = B_SPLINE_CURVE_WITH_KNOTS ( 'NONE', 3,
 ( #8905, #21313, #4936, #23243 ),
 .UNSPECIFIED., .F., .F.,
 ( 4, 4 ),
 ( 0.000000000000000000, 0.002452478801916361129 ),
 .UNSPECIFIED. ) ;
#22455 = CARTESIAN_POINT ( 'NONE',  ( 4.000000000000000000, 4.898587196589412829E-16, 1.925000002731188209 ) ) ;
#22456 = ORIENTED_EDGE ( 'NONE', *, *, #13903, .F. ) ;
#22457 = LINE ( 'NONE', #22702, #22894 ) ;
#22458 = VECTOR ( 'NONE', #17818, 1000.000000000000000 ) ;
#22459 = CARTESIAN_POINT ( 'NONE',  ( 65.70000000218495018, 8.232233047033629347, 13.23223304703362402 ) ) ;
#22460 = EDGE_CURVE ( 'NONE', #17999, #6426, #4842, .T. ) ;
#22461 = CARTESIAN_POINT ( 'NONE',  ( 4.000000000000001776, -1.656854249492379694, 19.43750000000001066 ) ) ;
#22462 = ORIENTED_EDGE ( 'NONE', *, *, #13673, .T. ) ;
#22463 = CARTESIAN_POINT ( 'NONE',  ( 18.14354716966726144, -11.25000000000000355, 5.000000000000079936 ) ) ;
#22464 = ORIENTED_EDGE ( 'NONE', *, *, #20012, .T. ) ;
#22465 = CARTESIAN_POINT ( 'NONE',  ( -3.999999999999999112, 1.656854249492380804, 12.06250000273119838 ) ) ;
#22466 = AXIS2_PLACEMENT_3D ( 'NONE', #13164, #16869, #14728 ) ;
#22467 = CARTESIAN_POINT ( 'NONE',  ( 4.000000000000000000, 1.656854249492381248, -0.01249999726881388488 ) ) ;
#22468 = CARTESIAN_POINT ( 'NONE',  ( 54.28125000000000000, 8.343145750507600766, 11.00000000000000533 ) ) ;
#22469 = CARTESIAN_POINT ( 'NONE',  ( -11.84783529071655295, -8.974600000000002353, 5.000000000000079936 ) ) ;
#22470 = CARTESIAN_POINT ( 'NONE',  ( -1.432654583217639610, -3.458734124999999882, 17.62500000136560274 ) ) ;
#22471 = CARTESIAN_POINT ( 'NONE',  ( 37.81203609676620658, -9.000000000000003553, 5.000000000000079936 ) ) ;
#22472 = AXIS2_PLACEMENT_3D ( 'NONE', #10019, #17306, #411 ) ;
#22473 = AXIS2_PLACEMENT_3D ( 'NONE', #19306, #12155, #19423 ) ;
#22474 = CARTESIAN_POINT ( 'NONE',  ( -66.50000000109245946, 12.06698729999999919, 15.85617417291294196 ) ) ;
#22475 = EDGE_LOOP ( 'NONE', ( #4874, #5007, #19548, #304 ) ) ;
#22476 = CARTESIAN_POINT ( 'NONE',  ( 72.50000000000000000, 9.999999999999998224, 12.49999999999999289 ) ) ;
#22477 = VERTEX_POINT ( 'NONE', #6767 ) ;
#22478 = PLANE ( 'NONE',  #5579 ) ;
#22479 = CARTESIAN_POINT ( 'NONE',  ( -70.84999999999998010, 11.03553390593276973, 17.49999999999997158 ) ) ;
#22480 = ORIENTED_EDGE ( 'NONE', *, *, #19049, .F. ) ;
#22481 = CYLINDRICAL_SURFACE ( 'NONE', #15897, 5.000000000000011546 ) ;
#22482 = AXIS2_PLACEMENT_3D ( 'NONE', #20131, #18363, #9641 ) ;
#22483 = CARTESIAN_POINT ( 'NONE',  ( 22.71892870323381786, -9.000000000000003553, 5.000000000000079936 ) ) ;
#22484 = CARTESIAN_POINT ( 'NONE',  ( -6.123233995736766085E-15, 0.000000000000000000, -50.00000000000000000 ) ) ;
#22485 = PLANE ( 'NONE',  #2184 ) ;
#22486 = VERTEX_POINT ( 'NONE', #22687 ) ;
#22487 = CARTESIAN_POINT ( 'NONE',  ( 4.000000000000000000, 4.898587196589412829E-16, 0.8000000000000020428 ) ) ;
#22488 = ORIENTED_EDGE ( 'NONE', *, *, #5404, .F. ) ;
#22489 =( GEOMETRIC_REPRESENTATION_CONTEXT ( 3 ) GLOBAL_UNCERTAINTY_ASSIGNED_CONTEXT ( ( #8588 ) ) GLOBAL_UNIT_ASSIGNED_CONTEXT ( ( #14527, #21546, #22015 ) ) REPRESENTATION_CONTEXT ( 'NONE', 'WORKASPACE' ) );
#22490 = CARTESIAN_POINT ( 'NONE',  ( 1.656854249492384135, -3.999999999999999112, 15.31250000000000888 ) ) ;
#22491 = CARTESIAN_POINT ( 'NONE',  ( 0.000000000000000000, 0.000000000000000000, 0.000000000000000000 ) ) ;
#22492 = EDGE_CURVE ( 'NONE', #7460, #13757, #12302, .T. ) ;
#22493 = VECTOR ( 'NONE', #12215, 1000.000000000000000 ) ;
#22494 = ORIENTED_EDGE ( 'NONE', *, *, #16247, .T. ) ;
#22495 = FACE_OUTER_BOUND ( 'NONE', #3627, .T. ) ;
#22496 = MECHANICAL_DESIGN_GEOMETRIC_PRESENTATION_REPRESENTATION (  '', ( #18679 ), #8742 ) ;
#22497 = ADVANCED_FACE ( 'NONE', ( #4618 ), #2560, .T. ) ;
#22498 = CARTESIAN_POINT ( 'NONE',  ( -3.999999999999999112, 0.000000000000000000, 18.12500000273119483 ) ) ;
#22499 = CARTESIAN_POINT ( 'NONE',  ( 70.20000000109246230, 9.143825827087052716, 12.93301269999999192 ) ) ;
#22500 = ORIENTED_EDGE ( 'NONE', *, *, #22940, .F. ) ;
#22501 = CARTESIAN_POINT ( 'NONE',  ( 5.969670414742682674, 4.058962678540098956, -0.4037800551813739425 ) ) ;
#22502 = DIRECTION ( 'NONE',  ( 0.000000000000000000, 0.5877852522924685852, 0.8090169943749506709 ) ) ;
#22503 = VECTOR ( 'NONE', #21798, 1000.000000000000000 ) ;
#22504 = EDGE_CURVE ( 'NONE', #8139, #7387, #782, .T. ) ;
#22505 = CARTESIAN_POINT ( 'NONE',  ( 69.00000000109245946, 10.85617417291294551, 17.06698729999999742 ) ) ;
#22506 = CARTESIAN_POINT ( 'NONE',  ( 3.458734125000001214, 1.432654583217640498, 15.00000000136560629 ) ) ;
#22507 = DIRECTION ( 'NONE',  ( -1.000000000000000000, 0.000000000000000000, 0.000000000000000000 ) ) ;
#22508 = AXIS2_PLACEMENT_3D ( 'NONE', #16280, #12711, #19963 ) ;
#22509 = LINE ( 'NONE', #8164, #16496 ) ;
#22510 = CARTESIAN_POINT ( 'NONE',  ( -4.000000000000000000, -1.656854249492383246, 3.362500000000005151 ) ) ;
#22511 = DIRECTION ( 'NONE',  ( -1.224646799147353207E-16, 0.000000000000000000, -1.000000000000000000 ) ) ;
#22512 = CARTESIAN_POINT ( 'NONE',  ( -2.445694354108819191, 2.445694354108820523, 11.31250000136560452 ) ) ;
#22513 = CARTESIAN_POINT ( 'NONE',  ( 2.499999999999999556, -10.90201369670497655, -1.464956435139657343 ) ) ;
#22514 = PRODUCT_DEFINITION_SHAPE ( 'NONE', 'NONE',  #6539 ) ;
#22515 = ORIENTED_EDGE ( 'NONE', *, *, #1201, .F. ) ;
#22516 = LINE ( 'NONE', #6957, #2856 ) ;
#22517 = VERTEX_POINT ( 'NONE', #22929 ) ;
#22518 = CARTESIAN_POINT ( 'NONE',  ( 58.31250000000000000, 14.00000000000000000, 14.99999999999997691 ) ) ;
#22519 = CARTESIAN_POINT ( 'NONE',  ( -67.70000000109246230, 7.933012699999995476, 14.14382582708705094 ) ) ;
#22520 = SHAPE_DEFINITION_REPRESENTATION ( #3758, #21657 ) ;
#22521 = VECTOR ( 'NONE', #3824, 1000.000000000000000 ) ;
#22522 = ORIENTED_EDGE ( 'NONE', *, *, #3069, .T. ) ;
#22523 = CARTESIAN_POINT ( 'NONE',  ( 50.00000000000000000, -10.00000000000001954, 15.00000000000002842 ) ) ;
#22524 = ORIENTED_EDGE ( 'NONE', *, *, #14062, .F. ) ;
#22525 = AXIS2_PLACEMENT_3D ( 'NONE', #3460, #16050, #19734 ) ;
#22526 = EDGE_CURVE ( 'NONE', #15893, #10715, #13617, .T. ) ;
#22527 = VERTEX_POINT ( 'NONE', #21230 ) ;
#22528 = CARTESIAN_POINT ( 'NONE',  ( 1.432654583217641386, 3.458734125000000770, 16.37500000136560629 ) ) ;
#22529 = AXIS2_PLACEMENT_3D ( 'NONE', #1179, #3100, #21275 ) ;
#22530 = CARTESIAN_POINT ( 'NONE',  ( 56.43750000000000000, 10.00000000000000711, 17.99999999999999645 ) ) ;
#22531 = VECTOR ( 'NONE', #15817, 1000.000000000000000 ) ;
#22532 = CARTESIAN_POINT ( 'NONE',  ( -68.65000000109247935, 12.06698730000000097, 14.99999999999999645 ) ) ;
#22533 = EDGE_CURVE ( 'NONE', #6221, #2584, #15326, .T. ) ;
#22534 = CARTESIAN_POINT ( 'NONE',  ( 68.00000000109247367, 10.85617417291294551, 17.06698730000000097 ) ) ;
#22535 = B_SPLINE_CURVE_WITH_KNOTS ( 'NONE', 3,
 ( #5111, #5226, #3436, #10777, #23071, #6682, #19481, #3080, #3311, #10422, #15908, #8719, #17702, #1265, #23185, #6797, #16027, #14118, #21381, #3190, #23315, #6924, #16493, #2093 ),
 .UNSPECIFIED., .F., .F.,
 ( 4, 2, 2, 2, 2, 2, 2, 2, 2, 2, 2, 4 ),
 ( 0.000000000000000000, 0.0009154863746717545282, 0.001373229562007631738, 0.001830972749343509056, 0.002746459124015263042, 0.003204202311351139927, 0.003661945498687016378, 0.004577431873358769714, 0.005035175060694646598, 0.005492918248030520881, 0.006408404622702273783, 0.007323890997374024950 ),
 .UNSPECIFIED. ) ;
#22536 = CARTESIAN_POINT ( 'NONE',  ( -71.95000000000001705, 7.499999999999995559, 13.96446609406725692 ) ) ;
#22537 = CIRCLE ( 'NONE', #5703, 8.749000000000002331 ) ;
#22538 = FACE_OUTER_BOUND ( 'NONE', #3327, .T. ) ;
#22539 = EDGE_CURVE ( 'NONE', #21943, #14331, #10148, .T. ) ;
#22540 = CARTESIAN_POINT ( 'NONE',  ( 54.24768183416157541, 7.830560233210222876, 17.07320092032950498 ) ) ;
#22541 = DIRECTION ( 'NONE',  ( -1.000000000000000000, 0.000000000000000000, 0.000000000000000000 ) ) ;
#22542 = ADVANCED_FACE ( 'NONE', ( #12062 ), #2917, .T. ) ;
#22543 = CARTESIAN_POINT ( 'NONE',  ( -3.458734125000000770, 1.432654583217640498, 2.925000001365598123 ) ) ;
#22544 = CARTESIAN_POINT ( 'NONE',  ( 2.445694354108821411, 2.445694354108820523, 11.06250000136560452 ) ) ;
#22545 = CARTESIAN_POINT ( 'NONE',  ( 4.000000000000000888, 1.656854249492381248, 12.68750000273119660 ) ) ;
#22546 = CIRCLE ( 'NONE', #13399, 9.000000000000023093 ) ;
#22547 = PLANE ( 'NONE',  #19110 ) ;
#22548 = AXIS2_PLACEMENT_3D ( 'NONE', #4131, #6051, #7981 ) ;
#22549 = EDGE_LOOP ( 'NONE', ( #20838, #12748, #8699, #13539 ) ) ;
#22550 = DIRECTION ( 'NONE',  ( -0.000000000000000000, -0.000000000000000000, 1.000000000000000000 ) ) ;
#22551 = VERTEX_POINT ( 'NONE', #4731 ) ;
#22552 = CARTESIAN_POINT ( 'NONE',  ( 51.18750000000000711, 9.999999999999989342, 11.99999999999999467 ) ) ;
#22553 =( NAMED_UNIT ( * ) SI_UNIT ( $, .STERADIAN. ) SOLID_ANGLE_UNIT ( ) );
#22554 = CARTESIAN_POINT ( 'NONE',  ( -2.445694354108820523, 2.445694354108820523, 1.612500001365596125 ) ) ;
#22555 = CARTESIAN_POINT ( 'NONE',  ( 2.445694354108820079, 2.445694354108820523, 0.3625000013655951259 ) ) ;
#22556 = ORIENTED_EDGE ( 'NONE', *, *, #2344, .F. ) ;
#22557 = CARTESIAN_POINT ( 'NONE',  ( 2.828427124746191179, 2.828427124746190291, 14.62500000000000888 ) ) ;
#22558 = CARTESIAN_POINT ( 'NONE',  ( 4.999999999999999112, 1.699438267350500409, -9.241976615262139205 ) ) ;
#22559 = VECTOR ( 'NONE', #15772, 1000.000000000000000 ) ;
#22560 = DIRECTION ( 'NONE',  ( 0.000000000000000000, -0.7071067811865406894, 0.7071067811865545671 ) ) ;
#22561 = ORIENTED_EDGE ( 'NONE', *, *, #16652, .T. ) ;
#22562 = CARTESIAN_POINT ( 'NONE',  ( -70.90000000218495302, 11.76776695296636888, 16.76776695296636532 ) ) ;
#22563 = EDGE_CURVE ( 'NONE', #18607, #12520, #19329, .T. ) ;
#22564 = CARTESIAN_POINT ( 'NONE',  ( 54.99999999999992895, 15.00000000000000000, 5.000000000000001776 ) ) ;
#22565 = VECTOR ( 'NONE', #2354, 1000.000000000000000 ) ;
#22566 = CARTESIAN_POINT ( 'NONE',  ( 4.000000000000000000, 0.000000000000000000, 19.04999999999996874 ) ) ;
#22567 = EDGE_CURVE ( 'NONE', #7262, #10320, #1900, .T. ) ;
#22568 = CYLINDRICAL_SURFACE ( 'NONE', #14093, 4.000000000000001776 ) ;
#22569 = EDGE_CURVE ( 'NONE', #18480, #23070, #8062, .T. ) ;
#22570 = FACE_OUTER_BOUND ( 'NONE', #16963, .T. ) ;
#22571 = AXIS2_PLACEMENT_3D ( 'NONE', #2721, #20561, #4166 ) ;
#22572 = CARTESIAN_POINT ( 'NONE',  ( 71.05000000109247082, 12.06698730000000097, 14.99999999999999645 ) ) ;
#22573 = EDGE_CURVE ( 'NONE', #15974, #22990, #7251, .T. ) ;
#22574 = CARTESIAN_POINT ( 'NONE',  ( 2.500000000000000000, -1.178949249685214307, 2.042000000000001592 ) ) ;
#22575 = VECTOR ( 'NONE', #17172, 1000.000000000000000 ) ;
#22576 = CARTESIAN_POINT ( 'NONE',  ( 53.28356816583845301, 8.689308171935074654, 12.02818770551464489 ) ) ;
#22577 = CARTESIAN_POINT ( 'NONE',  ( -1.432654583217640498, 3.458734125000000770, 3.800000001365595459 ) ) ;
#22578 = CARTESIAN_POINT ( 'NONE',  ( 1.872352939448454495E-15, -3.458734125000000770, 14.93750000136560452 ) ) ;
#22579 = FACE_OUTER_BOUND ( 'NONE', #15976, .T. ) ;
#22580 = CARTESIAN_POINT ( 'NONE',  ( -71.05000000109245661, 9.999999999999998224, 12.93301269999999192 ) ) ;
#22581 = DIRECTION ( 'NONE',  ( 0.000000000000000000, 0.000000000000000000, -1.000000000000000000 ) ) ;
#22582 = EDGE_LOOP ( 'NONE', ( #2922, #3973, #15190, #14385 ) ) ;
#22583 = PLANE ( 'NONE',  #11145 ) ;
#22584 =( BOUNDED_CURVE ( )  B_SPLINE_CURVE ( 2, ( #2338, #15307, #4261, #13144, #9551, #15068, #16848, #2561, #7513, #7861, #20408, #5698, #14955, #18864, #7986, #13032, #3893, #653, #2449, #426, #11229, #9428, #11597, #22324, #22580, #6184, #18503, #2090, #9671, #22206, #17079, #13504, #15184, #20769, #5939, #20529, #11478, #22444, #6057, #13388, #9784, #2808, #8340, #11952, #2695, #15658, #22930, #17558, #6543, #3045, #19103, #10268, #12177, #1123, #10036, #17673, #17324, #889, #2918, #21231, #22688, #6657, #17443, #19220, #8224, #13859, #21115, #8469, #13969, #8115, #19330, #20879, #15542, #11828, #8574, #4619, #15773, #783, #22807, #4732, #15425, #4488, #6300, #13618, #6419, #23045, #4843, #12063, #13734, #19448, #20999, #10393, #10149, #1235, #1008, #2118, #20318, #14538, #9453, #11512, #7779, #2364, #11621, #2476, #5734, #456, #20683, #13173, #3491, #21803, #5285, #4165, #18892, #23608, #9811, #22474, #7890, #17104, #7097, #21676, #19890, #15208, #14414, #12630, #18531, #18784, #13063, #15097, #9697 ),
 .UNSPECIFIED., .F., .F. ) 
 B_SPLINE_CURVE_WITH_KNOTS ( ( 3, 2, 2, 2, 2, 2, 2, 2, 2, 2, 2, 2, 2, 2, 2, 2, 2, 2, 2, 2, 2, 2, 2, 2, 2, 2, 2, 2, 2, 2, 2, 2, 2, 2, 2, 2, 2, 2, 2, 2, 2, 2, 2, 2, 2, 2, 2, 2, 2, 2, 2, 2, 2, 2, 2, 2, 2, 2, 2, 2, 2, 2, 2, 2, 3 ),
 ( 0.000000000000000000, 0.01562500000000000000, 0.03125000000000000000, 0.04687500000000000000, 0.06250000000000000000, 0.07812500000000000000, 0.09375000000000000000, 0.1093750000000000000, 0.1250000000000000000, 0.1406250000000000000, 0.1562500000000000000, 0.1718750000000000000, 0.1875000000000000000, 0.2031250000000000000, 0.2187500000000000000, 0.2343750000000000000, 0.2500000000000000000, 0.2656250000000000000, 0.2812500000000000000, 0.2968750000000000000, 0.3125000000000000000, 0.3281250000000000000, 0.3437500000000000000, 0.3593750000000000000, 0.3750000000000000000, 0.3906250000000000000, 0.4062500000000000000, 0.4218750000000000000, 0.4375000000000000000, 0.4531250000000000000, 0.4687500000000000000, 0.4843750000000000000, 0.5000000000000000000, 0.5156250000000000000, 0.5312500000000000000, 0.5468750000000000000, 0.5625000000000000000, 0.5781250000000000000, 0.5937500000000000000, 0.6093750000000000000, 0.6250000000000000000, 0.6406250000000000000, 0.6562500000000000000, 0.6718750000000000000, 0.6875000000000000000, 0.7031250000000000000, 0.7187500000000000000, 0.7343750000000000000, 0.7500000000000000000, 0.7656250000000000000, 0.7812500000000000000, 0.7968750000000000000, 0.8125000000000000000, 0.8281250000000000000, 0.8437500000000000000, 0.8593750000000000000, 0.8750000000000000000, 0.8906250000000000000, 0.9062500000000000000, 0.9218750000000000000, 0.9375000000000000000, 0.9531250000000000000, 0.9687500000000000000, 0.9843750000000000000, 1.000000000000000000 ),
 .UNSPECIFIED. ) 
 CURVE ( )  GEOMETRIC_REPRESENTATION_ITEM ( )  RATIONAL_B_SPLINE_CURVE ( ( 1.000000000000000000, 0.9238795325112867385, 1.000000000000000000, 0.9238795325112867385, 1.000000000000000000, 0.9238795325112867385, 1.000000000000000000, 0.9238795325112867385, 1.000000000000000000, 0.9238795325112867385, 1.000000000000000000, 0.9238795325112867385, 1.000000000000000000, 0.9238795325112867385, 1.000000000000000000, 0.9238795325112867385, 1.000000000000000000, 0.9238795325112867385, 1.000000000000000000, 0.9238795325112867385, 1.000000000000000000, 0.9238795325112867385, 1.000000000000000000, 0.9238795325112867385, 1.000000000000000000, 0.9238795325112867385, 1.000000000000000000, 0.9238795325112867385, 1.000000000000000000, 0.9238795325112867385, 1.000000000000000000, 0.9238795325112867385, 1.000000000000000000, 0.9238795325112867385, 1.000000000000000000, 0.9238795325112867385, 1.000000000000000000, 0.9238795325112867385, 1.000000000000000000, 0.9238795325112867385, 1.000000000000000000, 0.9238795325112867385, 1.000000000000000000, 0.9238795325112867385, 1.000000000000000000, 0.9238795325112867385, 1.000000000000000000, 0.9238795325112867385, 1.000000000000000000, 0.9238795325112867385, 1.000000000000000000, 0.9238795325112867385, 1.000000000000000000, 0.9238795325112867385, 1.000000000000000000, 0.9238795325112867385, 1.000000000000000000, 0.9238795325112867385, 1.000000000000000000, 0.9238795325112867385, 1.000000000000000000, 0.9238795325112867385, 1.000000000000000000, 0.9238795325112867385, 1.000000000000000000, 0.9238795325112867385, 1.000000000000000000, 0.9238795325112867385, 1.000000000000000000, 0.9238795325112867385, 1.000000000000000000, 0.9238795325112867385, 1.000000000000000000, 0.9238795325112867385, 1.000000000000000000, 0.9238795325112867385, 1.000000000000000000, 0.9238795325112867385, 1.000000000000000000, 0.9238795325112867385, 1.000000000000000000, 0.9238795325112867385, 1.000000000000000000, 0.9238795325112867385, 1.000000000000000000, 0.9238795325112867385, 1.000000000000000000, 0.9238795325112867385, 1.000000000000000000, 0.9238795325112867385, 1.000000000000000000, 0.9238795325112867385, 1.000000000000000000, 0.9238795325112867385, 1.000000000000000000, 0.9238795325112867385, 1.000000000000000000, 0.9238795325112867385, 1.000000000000000000, 0.9238795325112867385, 1.000000000000000000, 0.9238795325112867385, 1.000000000000000000, 0.9238795325112867385, 1.000000000000000000, 0.9238795325112867385, 1.000000000000000000, 0.9238795325112867385, 1.000000000000000000, 0.9238795325112867385, 1.000000000000000000, 0.9238795325112867385, 1.000000000000000000, 0.9238795325112867385, 1.000000000000000000, 0.9238795325112867385, 1.000000000000000000, 0.9238795325112867385, 1.000000000000000000, 0.9238795325112867385, 1.000000000000000000, 0.9238795325112867385, 1.000000000000000000, 0.9238795325112867385, 1.000000000000000000, 0.9238795325112867385, 1.000000000000000000, 0.9238795325112867385, 1.000000000000000000 ) ) 
 REPRESENTATION_ITEM ( '' )  );
#22585 = CARTESIAN_POINT ( 'NONE',  ( 4.000000000000000000, 1.656854249492381248, 3.987500002731185766 ) ) ;
#22586 = CARTESIAN_POINT ( 'NONE',  ( -70.70000000109247651, 7.933012699999995476, 14.14382582708705094 ) ) ;
#22587 = ORIENTED_EDGE ( 'NONE', *, *, #6763, .T. ) ;
#22588 = ORIENTED_EDGE ( 'NONE', *, *, #5984, .F. ) ;
#22589 = CARTESIAN_POINT ( 'NONE',  ( 4.999999999999999112, 1.699438267350372067, 9.241976615262164074 ) ) ;
#22590 = CARTESIAN_POINT ( 'NONE',  ( 0.000000000000000000, -6.772677083992425295, 5.538577986808878251 ) ) ;
#22591 = ORIENTED_EDGE ( 'NONE', *, *, #5834, .T. ) ;
#22592 = CARTESIAN_POINT ( 'NONE',  ( 4.175648173966055587, -2.207990556236547608, -3.469390959564065291 ) ) ;
#22593 = VECTOR ( 'NONE', #12496, 1000.000000000000000 ) ;
#22594 = VECTOR ( 'NONE', #10212, 1000.000000000000000 ) ;
#22595 = CARTESIAN_POINT ( 'NONE',  ( 67.85000000109248219, 12.06698730000000097, 14.99999999999999645 ) ) ;
#22596 = CARTESIAN_POINT ( 'NONE',  ( 68.25000000109245946, 9.999999999999998224, 17.06698730000000097 ) ) ;
#22597 = ADVANCED_FACE ( 'NONE', ( #9176, #23513 ), #5548, .F. ) ;
#22598 = ORIENTED_EDGE ( 'NONE', *, *, #18002, .F. ) ;
#22599 = CARTESIAN_POINT ( 'NONE',  ( 0.000000000000000000, 0.000000000000000000, 19.04999999999996874 ) ) ;
#22600 = CARTESIAN_POINT ( 'NONE',  ( 57.75000000000000000, 7.171572875253819923, 17.82842712474619873 ) ) ;
#22601 = CARTESIAN_POINT ( 'NONE',  ( 0.000000000000000000, 8.734705317681626724, -0.4999240074894757413 ) ) ;
#22602 = CARTESIAN_POINT ( 'NONE',  ( -1.432654583217639610, -3.458734124999999882, 18.62500000136560629 ) ) ;
#22603 = AXIS2_PLACEMENT_3D ( 'NONE', #21409, #17727, #14266 ) ;
#22604 = PLANE ( 'NONE',  #575 ) ;
#22605 = CARTESIAN_POINT ( 'NONE',  ( 45.00000000000000000, -2.399706452296352932, 60.00000000000021316 ) ) ;
#22606 = ORIENTED_EDGE ( 'NONE', *, *, #2528, .T. ) ;
#22607 = LINE ( 'NONE', #17106, #763 ) ;
#22608 = LINE ( 'NONE', #17472, #601 ) ;
#22609 = CARTESIAN_POINT ( 'NONE',  ( 4.999999999999999112, -7.593217523260637591, 7.958834565716740528 ) ) ;
#22610 = ORIENTED_EDGE ( 'NONE', *, *, #13935, .F. ) ;
#22611 = CARTESIAN_POINT ( 'NONE',  ( 5.200000000000002842, 0.000000000000000000, -2.700000000000000622 ) ) ;
#22612 = DIRECTION ( 'NONE',  ( 0.3420201433256622736, 0.9396926207859106484, 0.000000000000000000 ) ) ;
#22613 = DIRECTION ( 'NONE',  ( 0.000000000000000000, 0.9510565162951545304, -0.3090169943749446757 ) ) ;
#22614 = LINE ( 'NONE', #13780, #15989 ) ;
#22615 = VERTEX_POINT ( 'NONE', #1596 ) ;
#22616 = FACE_BOUND ( 'NONE', #16741, .T. ) ;
#22617 = VERTEX_POINT ( 'NONE', #7373 ) ;
#22618 = CARTESIAN_POINT ( 'NONE',  ( 71.00000000109248788, 12.06698729999999919, 14.14382582708705094 ) ) ;
#22619 = CARTESIAN_POINT ( 'NONE',  ( 2.828427124746192067, -2.828427124746189847, 15.37500000000001066 ) ) ;
#22620 = CARTESIAN_POINT ( 'NONE',  ( 70.50000000218494733, 8.232233047033629347, 13.23223304703362402 ) ) ;
#22621 =( REPRESENTATION_RELATIONSHIP ('NONE','NONE', #8403, #1939 ) REPRESENTATION_RELATIONSHIP_WITH_TRANSFORMATION ( #17387 )SHAPE_REPRESENTATION_RELATIONSHIP( ) );
#22622 = ORIENTED_EDGE ( 'NONE', *, *, #16422, .T. ) ;
#22623 = CARTESIAN_POINT ( 'NONE',  ( 1.799999999999996048, 0.000000000000000000, 0.000000000000000000 ) ) ;
#22624 = SURFACE_STYLE_USAGE ( .BOTH. , #5753 ) ;
#22625 = CARTESIAN_POINT ( 'NONE',  ( 72.05000000109245661, 12.06698730000000097, 14.99999999999999645 ) ) ;
#22626 = EDGE_LOOP ( 'NONE', ( #14718, #2013, #3175, #3113 ) ) ;
#22627 = DIRECTION ( 'NONE',  ( 0.000000000000000000, -0.000000000000000000, 1.000000000000000000 ) ) ;
#22628 = FACE_BOUND ( 'NONE', #277, .T. ) ;
#22629 = CARTESIAN_POINT ( 'NONE',  ( 71.45000000109247651, 9.999999999999998224, 17.06698730000000097 ) ) ;
#22630 = CARTESIAN_POINT ( 'NONE',  ( 1.432654583217643163, -3.458734124999999437, 11.75000000136560629 ) ) ;
#22631 = CARTESIAN_POINT ( 'NONE',  ( 40.96287359071656908, -8.974600000000002353, 5.000000000000079936 ) ) ;
#22632 = CARTESIAN_POINT ( 'NONE',  ( 6.499999999999999112, 2.531211054341943711, -0.2595069192555981008 ) ) ;
#22633 = ORIENTED_EDGE ( 'NONE', *, *, #13752, .T. ) ;
#22634 = CARTESIAN_POINT ( 'NONE',  ( -1.656854249492380804, 4.000000000000000000, 3.112500000000002487 ) ) ;
#22635 = DIRECTION ( 'NONE',  ( 0.000000000000000000, -0.4999999999999993339, 0.8660254037844390407 ) ) ;
#22636 = CARTESIAN_POINT ( 'NONE',  ( 3.458734125000002102, -1.432654583217639610, 10.87500000136560452 ) ) ;
#22637 = DIRECTION ( 'NONE',  ( -1.000000000000000000, -0.000000000000000000, -0.000000000000000000 ) ) ;
#22638 = EDGE_LOOP ( 'NONE', ( #4755, #10628, #10998, #936 ) ) ;
#22639 = ADVANCED_FACE ( 'NONE', ( #21833 ), #5435, .F. ) ;
#22640 = CARTESIAN_POINT ( 'NONE',  ( -66.40000000109247935, 10.85617417291294551, 17.06698730000000097 ) ) ;
#22641 = EDGE_LOOP ( 'NONE', ( #1237, #14883, #18638, #11573, #10999, #17218 ) ) ;
#22642 = CARTESIAN_POINT ( 'NONE',  ( -66.80000000109247082, 7.933012699999995476, 15.85617417291294196 ) ) ;
#22643 = ORIENTED_EDGE ( 'NONE', *, *, #6439, .T. ) ;
#22644 = CARTESIAN_POINT ( 'NONE',  ( -6.989194030332740226, -11.25000000000000355, 5.000000000000079936 ) ) ;
#22645 = ORIENTED_EDGE ( 'NONE', *, *, #12659, .F. ) ;
#22646 = ORIENTED_EDGE ( 'NONE', *, *, #21192, .F. ) ;
#22647 = CARTESIAN_POINT ( 'NONE',  ( 2.445694354108821411, 2.445694354108820523, 16.31250000136560629 ) ) ;
#22648 = EDGE_CURVE ( 'NONE', #10047, #22418, #20023, .T. ) ;
#22649 = CARTESIAN_POINT ( 'NONE',  ( 54.65625000000001421, 7.000000000000003553, 16.24264068711929099 ) ) ;
#22650 = CARTESIAN_POINT ( 'NONE',  ( -69.05000000109247082, 7.933012699999995476, 14.99999999999999645 ) ) ;
#22651 = CARTESIAN_POINT ( 'NONE',  ( 68.05000000109247082, 9.999999999999998224, 17.06698730000000097 ) ) ;
#22652 = CARTESIAN_POINT ( 'NONE',  ( -71.89999999999999147, 7.499999999999996447, 14.99999999999999645 ) ) ;
#22653 = PLANE ( 'NONE',  #18364 ) ;
#22654 = CARTESIAN_POINT ( 'NONE',  ( 58.65393183416157541, 6.971812294485357775, 16.17458954617365663 ) ) ;
#22655 = CARTESIAN_POINT ( 'NONE',  ( 0.000000000000000000, 9.915734732513218574, 4.762163868918309007 ) ) ;
#22656 = CARTESIAN_POINT ( 'NONE',  ( -2.445694354108819635, -2.445694354108820967, 3.112500001365597679 ) ) ;
#22657 = CYLINDRICAL_SURFACE ( 'NONE', #10072, 11.00000000000000000 ) ;
#22658 = CARTESIAN_POINT ( 'NONE',  ( 4.000000000000001776, -1.656854249492379694, 10.56250000273119660 ) ) ;
#22659 = CARTESIAN_POINT ( 'NONE',  ( -72.50000000000000000, 9.999999999999998224, 17.49999999999999645 ) ) ;
#22660 = ORIENTED_EDGE ( 'NONE', *, *, #9397, .F. ) ;
#22661 = EDGE_CURVE ( 'NONE', #19691, #16922, #1826, .T. ) ;
#22662 = FACE_OUTER_BOUND ( 'NONE', #9986, .T. ) ;
#22663 = EDGE_LOOP ( 'NONE', ( #8514, #3775, #2011, #10682 ) ) ;
#22664 = CARTESIAN_POINT ( 'NONE',  ( 59.21643183416158962, 12.97181229448535689, 16.31069182806490758 ) ) ;
#22665 = CARTESIAN_POINT ( 'NONE',  ( -2.117863837641485618E-16, 3.458734125000000326, 0.4875000013655952369 ) ) ;
#22666 = EDGE_CURVE ( 'NONE', #4211, #990, #4975, .T. ) ;
#22667 = CARTESIAN_POINT ( 'NONE',  ( 3.458734125000000326, 4.235727675282971730E-16, 1.237500001365595903 ) ) ;
#22668 = VERTEX_POINT ( 'NONE', #8936 ) ;
#22669 = CARTESIAN_POINT ( 'NONE',  ( -3.999999999999998224, -1.656854249492383246, 15.06250000000001066 ) ) ;
#22670 = DIRECTION ( 'NONE',  ( -1.000000000000000000, 0.000000000000000000, 0.000000000000000000 ) ) ;
#22671 = ORIENTED_EDGE ( 'NONE', *, *, #20791, .F. ) ;
#22672 = ADVANCED_FACE ( 'NONE', ( #10503 ), #2655, .T. ) ;
#22673 = EDGE_CURVE ( 'NONE', #14810, #4086, #21932, .T. ) ;
#22674 = CARTESIAN_POINT ( 'NONE',  ( -71.35000000218494165, 8.964466094067258695, 12.49999999999999289 ) ) ;
#22675 = CARTESIAN_POINT ( 'NONE',  ( 1.432654583217640276, 3.458734125000000770, -1.324999998634403209 ) ) ;
#22676 = CARTESIAN_POINT ( 'NONE',  ( -5.434916218090831919, -4.367703157927335766, -3.442152416367926460 ) ) ;
#22677 = DIRECTION ( 'NONE',  ( 0.000000000000000000, 0.000000000000000000, 1.000000000000000000 ) ) ;
#22678 = DIRECTION ( 'NONE',  ( -1.000000000000000000, -0.000000000000000000, -0.000000000000000000 ) ) ;
#22679 = CARTESIAN_POINT ( 'NONE',  ( 69.90000000109247935, 7.933012699999995476, 14.14382582708705094 ) ) ;
#22680 = VECTOR ( 'NONE', #13861, 1000.000000000000114 ) ;
#22681 = CARTESIAN_POINT ( 'NONE',  ( -19.99999999999999645, -9.000000000000003553, 5.000000000000079936 ) ) ;
#22682 = CARTESIAN_POINT ( 'NONE',  ( 56.65856816583844591, 7.028187705514647554, 16.31069182806492179 ) ) ;
#22683 = VECTOR ( 'NONE', #10229, 999.9999999999997726 ) ;
#22684 = EDGE_CURVE ( 'NONE', #11604, #9577, #6888, .T. ) ;
#22685 = CARTESIAN_POINT ( 'NONE',  ( -3.458734125000000770, 1.432654583217640498, 5.925000001365596347 ) ) ;
#22686 = CARTESIAN_POINT ( 'NONE',  ( 1.432654583217641386, 3.458734125000000770, 12.37500000136560629 ) ) ;
#22687 = CARTESIAN_POINT ( 'NONE',  ( -1.506022603841227436, 0.000000000000000000, -8.265000000000021885 ) ) ;
#22688 = CARTESIAN_POINT ( 'NONE',  ( -69.25000000109245946, 7.933012699999995476, 14.99999999999999645 ) ) ;
#22689 = DIRECTION ( 'NONE',  ( -4.930380657631312836E-32, -0.3420201433256691015, -0.9396926207859083169 ) ) ;
#22690 = CARTESIAN_POINT ( 'NONE',  ( 65.75000000218494733, 8.964466094067219615, 12.50000000000003553 ) ) ;
#22691 = ORIENTED_EDGE ( 'NONE', *, *, #7350, .T. ) ;
#22692 = CARTESIAN_POINT ( 'NONE',  ( -4.141042297810615835, 2.227970268150415656, -3.687027686973619822 ) ) ;
#22693 = DIRECTION ( 'NONE',  ( 0.000000000000000000, 0.000000000000000000, 1.000000000000000000 ) ) ;
#22694 = EDGE_CURVE ( 'NONE', #7612, #10715, #1506, .T. ) ;
#22695 = AXIS2_PLACEMENT_3D ( 'NONE', #71, #18275, #1860 ) ;
#22696 = ORIENTED_EDGE ( 'NONE', *, *, #5457, .F. ) ;
#22697 = ORIENTED_EDGE ( 'NONE', *, *, #8079, .T. ) ;
#22698 = CARTESIAN_POINT ( 'NONE',  ( -65.00000000000000000, 15.00000000000000000, 10.00000000000008882 ) ) ;
#22699 = CARTESIAN_POINT ( 'NONE',  ( 52.21875000000001421, 14.00000000000001066, 16.65685424949235482 ) ) ;
#22700 = VERTEX_POINT ( 'NONE', #1708 ) ;
#22701 = EDGE_CURVE ( 'NONE', #23136, #17296, #5318, .T. ) ;
#22702 = CARTESIAN_POINT ( 'NONE',  ( -19.99999999999999645, -9.000000000000003553, 5.000000000000079936 ) ) ;
#22703 = ADVANCED_FACE ( 'NONE', ( #9051 ), #22547, .F. ) ;
#22704 = AXIS2_PLACEMENT_3D ( 'NONE', #8216, #10028, #6411 ) ;
#22705 = PRODUCT_DEFINITION_CONTEXT ( 'detailed design', #5946, 'design' ) ;
#22706 = CARTESIAN_POINT ( 'NONE',  ( 69.85000000109248219, 7.933012699999995476, 14.99999999999999645 ) ) ;
#22707 = CARTESIAN_POINT ( 'NONE',  ( 69.75000000109245946, 11.46158073645647235, 16.46158073645647235 ) ) ;
#22708 = PRODUCT_DEFINITION_SHAPE ( 'NONE', 'NONE',  #3726 ) ;
#22709 = ORIENTED_EDGE ( 'NONE', *, *, #3476, .F. ) ;
#22710 = FACE_OUTER_BOUND ( 'NONE', #8550, .T. ) ;
#22711 =( BOUNDED_CURVE ( )  B_SPLINE_CURVE ( 2, ( #9740, #19279, #2521, #20837, #13686, #8418, #8064, #2757, #22402 ),
 .UNSPECIFIED., .F., .F. ) 
 B_SPLINE_CURVE_WITH_KNOTS ( ( 3, 2, 2, 2, 3 ),
 ( 0.6999999999999999556, 0.7125000000000000222, 0.7249999999999999778, 0.7375000000000000444, 0.7500000000000000000 ),
 .UNSPECIFIED. ) 
 CURVE ( )  GEOMETRIC_REPRESENTATION_ITEM ( )  RATIONAL_B_SPLINE_CURVE ( ( 1.000000000000000000, 0.9238795325112867385, 1.000000000000000000, 0.9238795325112867385, 1.000000000000000000, 0.9238795325112867385, 1.000000000000000000, 0.9238795325112867385, 1.000000000000000000 ) ) 
 REPRESENTATION_ITEM ( '' )  );
#22712 = CARTESIAN_POINT ( 'NONE',  ( 54.93750000000000711, 10.00000000000001776, 18.99999999999999645 ) ) ;
#22713 = CARTESIAN_POINT ( 'NONE',  ( 71.55000000218494449, 12.50000000000000000, 13.96446609406725692 ) ) ;
#22714 = CARTESIAN_POINT ( 'NONE',  ( 3.458734125000002102, -1.432654583217639610, 18.87500000136560629 ) ) ;
#22715 = DIRECTION ( 'NONE',  ( 1.224646799147353207E-16, -0.000000000000000000, 1.000000000000000000 ) ) ;
#22716 = CARTESIAN_POINT ( 'NONE',  ( -65.00000000000000000, -10.00000000000000178, 17.49999999999999645 ) ) ;
#22717 = EDGE_LOOP ( 'NONE', ( #12804, #9883 ) ) ;
#22718 = DIRECTION ( 'NONE',  ( -0.000000000000000000, -1.000000000000000000, -0.000000000000000000 ) ) ;
#22719 = CARTESIAN_POINT ( 'NONE',  ( -4.000000000000000000, 4.898587196589412829E-16, -3.699999999999998401 ) ) ;
#22720 = DIRECTION ( 'NONE',  ( -1.000000000000000000, -0.000000000000000000, -0.000000000000000000 ) ) ;
#22721 = VECTOR ( 'NONE', #19535, 1000.000000000000000 ) ;
#22722 = ORIENTED_EDGE ( 'NONE', *, *, #15139, .T. ) ;
#22723 = CARTESIAN_POINT ( 'NONE',  ( 4.154306624731137099, 2.398490048084935822, -3.721999068284414847 ) ) ;
#22724 = CARTESIAN_POINT ( 'NONE',  ( 1.489200000000000079, 0.000000000000000000, 0.000000000000000000 ) ) ;
#22725 = CARTESIAN_POINT ( 'NONE',  ( 49.55947366966726264, -11.25000000000000355, 5.000000000000079936 ) ) ;
#22726 = CONICAL_SURFACE ( 'NONE', #20422, 2.059999999999998721, 0.9599310885968738161 ) ;
#22727 = EDGE_CURVE ( 'NONE', #7848, #7815, #11082, .T. ) ;
#22728 = CARTESIAN_POINT ( 'NONE',  ( -70.90000000218495302, 11.76776695296636888, 16.76776695296636532 ) ) ;
#22729 = ORIENTED_EDGE ( 'NONE', *, *, #3220, .T. ) ;
#22730 = DIRECTION ( 'NONE',  ( 0.000000000000000000, -0.9510565162951500895, -0.3090169943749582204 ) ) ;
#22731 = VERTEX_POINT ( 'NONE', #22297 ) ;
#22732 = ADVANCED_FACE ( 'NONE', ( #20624 ), #20135, .T. ) ;
#22733 = CARTESIAN_POINT ( 'NONE',  ( -3.999999999999999112, 0.000000000000000000, 18.00000000000001066 ) ) ;
#22734 = VECTOR ( 'NONE', #3048, 1000.000000000000000 ) ;
#22735 = DIRECTION ( 'NONE',  ( -1.000000000000000000, 0.000000000000000000, 0.000000000000000000 ) ) ;
#22736 = CARTESIAN_POINT ( 'NONE',  ( 70.25000000218494733, 8.964466094067258695, 17.50000000000000355 ) ) ;
#22737 = CARTESIAN_POINT ( 'NONE',  ( -2.828427124746188515, -2.828427124746190735, 19.12500000000001066 ) ) ;
#22738 = DIRECTION ( 'NONE',  ( 0.000000000000000000, 0.000000000000000000, 1.000000000000000000 ) ) ;
#22739 = CARTESIAN_POINT ( 'NONE',  ( 67.55000000109247082, 8.538419263543522320, 16.46158073645647235 ) ) ;
#22740 = ORIENTED_EDGE ( 'NONE', *, *, #4635, .F. ) ;
#22741 = CARTESIAN_POINT ( 'NONE',  ( -27.50000000000000711, 4.500000000000003553, -36.31025403784446581 ) ) ;
#22742 = CARTESIAN_POINT ( 'NONE',  ( -3.999999999999999112, 0.000000000000000000, 19.00000000000001066 ) ) ;
#22743 = CARTESIAN_POINT ( 'NONE',  ( 69.30000000109247082, 7.933012699999995476, 14.14382582708705094 ) ) ;
#22744 = CARTESIAN_POINT ( 'NONE',  ( -1.432654583217638944, 3.458734125000000326, 13.25000000136560452 ) ) ;
#22745 = CARTESIAN_POINT ( 'NONE',  ( 25.00005080000000035, 0.000000000000000000, 0.000000000000000000 ) ) ;
#22746 = VECTOR ( 'NONE', #15456, 1000.000000000000000 ) ;
#22747 = DIRECTION ( 'NONE',  ( 1.000000000000000000, -0.000000000000000000, -0.000000000000000000 ) ) ;
#22748 = VERTEX_POINT ( 'NONE', #7727 ) ;
#22749 = CARTESIAN_POINT ( 'NONE',  ( -4.000000000000000888, 1.656854249492380804, 0.2375000000000018763 ) ) ;
#22750 = DIRECTION ( 'NONE',  ( 7.087422195345011518E-32, 1.000000000000000000, -0.000000000000000000 ) ) ;
#22751 = AXIS2_PLACEMENT_3D ( 'NONE', #22385, #4314, #11767 ) ;
#22752 = CARTESIAN_POINT ( 'NONE',  ( 3.458734125000001214, 1.432654583217640498, 11.00000000136560452 ) ) ;
#22753 = DIRECTION ( 'NONE',  ( 0.000000000000000000, 0.000000000000000000, 1.000000000000000000 ) ) ;
#22754 = ORIENTED_EDGE ( 'NONE', *, *, #13319, .F. ) ;
#22755 = LINE ( 'NONE', #15249, #15145 ) ;
#22756 = ORIENTED_EDGE ( 'NONE', *, *, #985, .T. ) ;
#22757 = CARTESIAN_POINT ( 'NONE',  ( -69.10000000109246798, 9.143825827087049163, 17.06698729999999742 ) ) ;
#22758 = ORIENTED_EDGE ( 'NONE', *, *, #13020, .T. ) ;
#22759 = CARTESIAN_POINT ( 'NONE',  ( 4.000000000000000000, 0.000000000000000000, 19.04999999999996874 ) ) ;
#22760 = VERTEX_POINT ( 'NONE', #2182 ) ;
#22761 =( REPRESENTATION_RELATIONSHIP ('NONE','NONE', #8403, #13579 ) REPRESENTATION_RELATIONSHIP_WITH_TRANSFORMATION ( #3721 )SHAPE_REPRESENTATION_RELATIONSHIP( ) );
#22762 = VERTEX_POINT ( 'NONE', #11570 ) ;
#22763 = CARTESIAN_POINT ( 'NONE',  ( 1.872352939448454495E-15, -3.458734125000000770, 12.93750000136560629 ) ) ;
#22764 = CARTESIAN_POINT ( 'NONE',  ( 45.00000000000000000, 10.00000000000001599, 15.00000000000003020 ) ) ;
#22765 = CARTESIAN_POINT ( 'NONE',  ( -68.00000000109247367, 10.85617417291294551, 17.06698729999999742 ) ) ;
#22766 = PRODUCT_RELATED_PRODUCT_CATEGORY ( 'part', '', ( #908 ) ) ;
#22767 = CARTESIAN_POINT ( 'NONE',  ( 65.85000000109248219, 7.933012699999995476, 14.99999999999999645 ) ) ;
#22768 = EDGE_CURVE ( 'NONE', #5706, #14730, #14937, .T. ) ;
#22769 = CARTESIAN_POINT ( 'NONE',  ( -67.10000000109246798, 10.85617417291294551, 12.93301269999999370 ) ) ;
#22770 = DIRECTION ( 'NONE',  ( 0.000000000000000000, 0.000000000000000000, 1.000000000000000000 ) ) ;
#22771 = CARTESIAN_POINT ( 'NONE',  ( 54.62268183416157541, 12.07320092032950676, 17.16943976678977180 ) ) ;
#22772 = CARTESIAN_POINT ( 'NONE',  ( 4.999999999999999112, 8.475820894092974456, 4.057423117305423155 ) ) ;
#22773 = CARTESIAN_POINT ( 'NONE',  ( -2.445694354108820523, 2.445694354108820523, 3.862500001365594571 ) ) ;
#22774 = DIRECTION ( 'NONE',  ( 0.000000000000000000, 0.000000000000000000, 1.000000000000000000 ) ) ;
#22775 = CARTESIAN_POINT ( 'NONE',  ( -3.999999999999999112, 0.000000000000000000, 11.12500000273119660 ) ) ;
#22776 = CARTESIAN_POINT ( 'NONE',  ( 4.999999999999999112, -3.174628368996134320, 8.152713396088753228 ) ) ;
#22777 = ORIENTED_EDGE ( 'NONE', *, *, #6663, .T. ) ;
#22778 = CARTESIAN_POINT ( 'NONE',  ( 46.41788101966725577, -11.25000000000000355, 5.000000000000079936 ) ) ;
#22779 = VERTEX_POINT ( 'NONE', #3742 ) ;
#22780 = CARTESIAN_POINT ( 'NONE',  ( 57.71643183416158251, 12.97181229448535689, 16.31069182806490758 ) ) ;
#22781 = AXIS2_PLACEMENT_3D ( 'NONE', #10457, #23221, #3351 ) ;
#22782 = DIRECTION ( 'NONE',  ( 0.000000000000000000, 0.000000000000000000, 1.000000000000000000 ) ) ;
#22783 = CARTESIAN_POINT ( 'NONE',  ( -2.445694354108819635, -2.445694354108820523, 0.8625000013655955700 ) ) ;
#22784 = AXIS2_PLACEMENT_3D ( 'NONE', #21027, #10178, #15686 ) ;
#22785 = CARTESIAN_POINT ( 'NONE',  ( 3.458734125000001214, -1.432654583217639610, -0.8249999986344029868 ) ) ;
#22786 = ORIENTED_EDGE ( 'NONE', *, *, #1612, .F. ) ;
#22787 = CYLINDRICAL_SURFACE ( 'NONE', #2593, 2.500000000000002220 ) ;
#22788 = LINE ( 'NONE', #19083, #18677 ) ;
#22789 = ORIENTED_EDGE ( 'NONE', *, *, #20402, .T. ) ;
#22790 = CARTESIAN_POINT ( 'NONE',  ( 2.000000000000008882, 3.464101615137749945, 0.000000000000000000 ) ) ;
#22791 = ORIENTED_EDGE ( 'NONE', *, *, #8067, .F. ) ;
#22792 = CARTESIAN_POINT ( 'NONE',  ( 56.47106816583845301, 6.971812294485350670, 13.82541045382635403 ) ) ;
#22793 = CARTESIAN_POINT ( 'NONE',  ( -69.45000000218493597, 8.964466094067258695, 17.50000000000000355 ) ) ;
#22794 = CARTESIAN_POINT ( 'NONE',  ( -2.445694354108820523, 2.445694354108820523, -3.137499998634402765 ) ) ;
#22795 = EDGE_CURVE ( 'NONE', #5860, #13392, #10516, .T. ) ;
#22796 = FACE_OUTER_BOUND ( 'NONE', #2225, .T. ) ;
#22797 = CARTESIAN_POINT ( 'NONE',  ( 66.09999999999999432, 9.999999999999998224, 17.49999999999999645 ) ) ;
#22798 = EDGE_CURVE ( 'NONE', #20481, #15099, #15275, .T. ) ;
#22799 = CARTESIAN_POINT ( 'NONE',  ( -71.20000000000000284, 8.232233047033629347, 13.23223304703362402 ) ) ;
#22800 = CARTESIAN_POINT ( 'NONE',  ( 69.35000000109248219, 11.46158073645647235, 13.53841926354352232 ) ) ;
#22801 = DIRECTION ( 'NONE',  ( 1.000000000000000000, 7.703719777548943412E-32, 0.000000000000000000 ) ) ;
#22802 = CARTESIAN_POINT ( 'NONE',  ( 52.81481816583844591, 12.99999999999999822, 14.93194885905435676 ) ) ;
#22803 = CARTESIAN_POINT ( 'NONE',  ( -3.458734125000000326, 1.432654583217640276, -2.324999998634404097 ) ) ;
#22804 = CARTESIAN_POINT ( 'NONE',  ( 1.025207404391860050E-15, 3.458734125000000770, 11.43750000136560452 ) ) ;
#22805 = EDGE_CURVE ( 'NONE', #2366, #633, #4108, .T. ) ;
#22806 =( LENGTH_UNIT ( ) NAMED_UNIT ( * ) SI_UNIT ( .MILLI., .METRE. ) );
#22807 = CARTESIAN_POINT ( 'NONE',  ( -68.35000000109246798, 8.538419263543522320, 16.46158073645647235 ) ) ;
#22808 = CARTESIAN_POINT ( 'NONE',  ( 4.211140560182196957, -2.431303136016555122, -3.745885042887436622 ) ) ;
#22809 = CARTESIAN_POINT ( 'NONE',  ( 65.50000000218494733, 8.232233047033627571, 16.76776695296636532 ) ) ;
#22810 = EDGE_LOOP ( 'NONE', ( #20359, #13527, #371, #4790 ) ) ;
#22811 = CARTESIAN_POINT ( 'NONE',  ( 3.999999999999999112, -0.7890432684750902093, -0.04868663549882291247 ) ) ;
#22812 = CARTESIAN_POINT ( 'NONE',  ( 7.347880794884118750E-16, -4.000000000000000000, 4.675000002731187543 ) ) ;
#22813 = ORIENTED_EDGE ( 'NONE', *, *, #1145, .F. ) ;
#22814 = ORIENTED_EDGE ( 'NONE', *, *, #16134, .F. ) ;
#22815 = CARTESIAN_POINT ( 'NONE',  ( -2.828427124746189403, -2.828427124746190735, 1.550000002731187765 ) ) ;
#22816 = FACE_OUTER_BOUND ( 'NONE', #22995, .T. ) ;
#22817 = ORIENTED_EDGE ( 'NONE', *, *, #21184, .F. ) ;
#22818 = CARTESIAN_POINT ( 'NONE',  ( 2.756197834950227410, 3.027510591568626896, -3.223146290109805356 ) ) ;
#22819 = EDGE_CURVE ( 'NONE', #16967, #22748, #18838, .T. ) ;
#22820 = CARTESIAN_POINT ( 'NONE',  ( 69.15000000109247935, 8.538419263543524096, 13.53841926354352054 ) ) ;
#22821 = AXIS2_PLACEMENT_3D ( 'NONE', #8316, #10373, #3144 ) ;
#22822 = CARTESIAN_POINT ( 'NONE',  ( 67.00000000109247367, 9.143825827087050939, 12.93301269999999370 ) ) ;
#22823 = EDGE_CURVE ( 'NONE', #3756, #19580, #7302, .T. ) ;
#22824 = ORIENTED_EDGE ( 'NONE', *, *, #11628, .T. ) ;
#22825 = CIRCLE ( 'NONE', #17864, 8.265000000000021885 ) ;
#22826 = DIRECTION ( 'NONE',  ( 0.000000000000000000, -0.8090169943749530024, 0.5877852522924653655 ) ) ;
#22827 = CARTESIAN_POINT ( 'NONE',  ( 57.93750000000000000, 10.00000000000001776, 18.99999999999999645 ) ) ;
#22828 = DIRECTION ( 'NONE',  ( 0.000000000000000000, 0.000000000000000000, -1.000000000000000000 ) ) ;
#22829 = EDGE_CURVE ( 'NONE', #7467, #15024, #2895, .T. ) ;
#22830 = CARTESIAN_POINT ( 'NONE',  ( 2.445694354108821855, -2.445694354108820079, 18.81250000136560629 ) ) ;
#22831 = CARTESIAN_POINT ( 'NONE',  ( 68.10000000218495586, 8.232233047033629347, 13.23223304703362402 ) ) ;
#22832 = EDGE_CURVE ( 'NONE', #11622, #735, #16929, .T. ) ;
#22833 = CIRCLE ( 'NONE', #8323, 8.265000000000021885 ) ;
#22834 = CARTESIAN_POINT ( 'NONE',  ( -1.799999999999996048, 0.000000000000000000, 0.000000000000000000 ) ) ;
#22835 = ORIENTED_EDGE ( 'NONE', *, *, #1306, .T. ) ;
#22836 = CARTESIAN_POINT ( 'NONE',  ( 3.851282720981234142, -0.3188430404951885788, 10.00000000000008882 ) ) ;
#22837 = DIRECTION ( 'NONE',  ( 1.000000000000000000, 7.703719777548943412E-32, 0.000000000000000000 ) ) ;
#22838 = CARTESIAN_POINT ( 'NONE',  ( -19.99999999999999645, -11.25000000000000355, 10.00000000000008882 ) ) ;
#22839 = VECTOR ( 'NONE', #19340, 1000.000000000000114 ) ;
#22840 = AXIS2_PLACEMENT_3D ( 'NONE', #4005, #11344, #20041 ) ;
#22841 = VERTEX_POINT ( 'NONE', #17052 ) ;
#22842 = CARTESIAN_POINT ( 'NONE',  ( 1.236993788156008760E-15, 0.000000000000000000, 21.31370849898476649 ) ) ;
#22843 = CARTESIAN_POINT ( 'NONE',  ( 2.500000000000000000, -1.178949249685218748, -2.041999999999998039 ) ) ;
#22844 = CARTESIAN_POINT ( 'NONE',  ( -60.00000000000000711, 9.999999999999998224, 20.00000000000001421 ) ) ;
#22845 = CARTESIAN_POINT ( 'NONE',  ( -70.75000000218496155, 12.50000000000000000, 13.96446609406725692 ) ) ;
#22846 = ORIENTED_EDGE ( 'NONE', *, *, #16827, .T. ) ;
#22847 = CARTESIAN_POINT ( 'NONE',  ( 3.250000000000004441, 5.629165124598849879, -3.700000000000000178 ) ) ;
#22848 = VERTEX_POINT ( 'NONE', #3870 ) ;
#22849 = CARTESIAN_POINT ( 'NONE',  ( 71.70000000109247651, 10.85617417291294551, 12.93301269999999192 ) ) ;
#22850 = CARTESIAN_POINT ( 'NONE',  ( 71.65000000218496723, 12.50000000000000000, 16.03553390593273420 ) ) ;
#22851 = AXIS2_PLACEMENT_3D ( 'NONE', #15588, #19148, #22854 ) ;
#22852 = CARTESIAN_POINT ( 'NONE',  ( 72.50000000000000000, 9.999999999999998224, 12.49999999999999289 ) ) ;
#22853 =( BOUNDED_CURVE ( )  B_SPLINE_CURVE ( 2, ( #4960, #12294, #3275, #23272, #3392, #8927, #3151, #6879, #1589 ),
 .UNSPECIFIED., .F., .F. ) 
 B_SPLINE_CURVE_WITH_KNOTS ( ( 3, 2, 2, 2, 3 ),
 ( 0.7500000000000000000, 0.7624999999999999556, 0.7750000000000000222, 0.7874999999999999778, 0.8000000000000000444 ),
 .UNSPECIFIED. ) 
 CURVE ( )  GEOMETRIC_REPRESENTATION_ITEM ( )  RATIONAL_B_SPLINE_CURVE ( ( 1.000000000000000000, 0.9238795325112867385, 1.000000000000000000, 0.9238795325112867385, 1.000000000000000000, 0.9238795325112867385, 1.000000000000000000, 0.9238795325112867385, 1.000000000000000000 ) ) 
 REPRESENTATION_ITEM ( '' )  );
#22854 = DIRECTION ( 'NONE',  ( 0.000000000000000000, -0.9510565162951500895, -0.3090169943749582204 ) ) ;
#22855 = CARTESIAN_POINT ( 'NONE',  ( 66.25000000109245946, 9.999999999999998224, 12.93301269999999192 ) ) ;
#22856 = ORIENTED_EDGE ( 'NONE', *, *, #19317, .F. ) ;
#22857 = AXIS2_PLACEMENT_3D ( 'NONE', #14997, #4057, #8795 ) ;
#22858 = DIRECTION ( 'NONE',  ( 0.000000000000000000, -0.000000000000000000, -1.000000000000000000 ) ) ;
#22859 = CARTESIAN_POINT ( 'NONE',  ( 2.499999999999999556, -9.680994141368733708, -5.222868219166961978 ) ) ;
#22860 = EDGE_CURVE ( 'NONE', #18371, #313, #11326, .T. ) ;
#22861 = CARTESIAN_POINT ( 'NONE',  ( 69.10000000109246798, 9.143825827087049163, 17.06698729999999742 ) ) ;
#22862 = CARTESIAN_POINT ( 'NONE',  ( 3.458734125000001214, 4.235727675282971730E-16, 12.93750000136560452 ) ) ;
#22863 = CARTESIAN_POINT ( 'NONE',  ( 0.000000000000000000, -4.057423117305452465, 8.475820894092962021 ) ) ;
#22864 = EDGE_CURVE ( 'NONE', #14597, #10607, #22315, .T. ) ;
#22865 = DIRECTION ( 'NONE',  ( 1.000000000000000000, -0.000000000000000000, -0.000000000000000000 ) ) ;
#22866 = VERTEX_POINT ( 'NONE', #20967 ) ;
#22867 = CARTESIAN_POINT ( 'NONE',  ( -2.325118450655084601, 2.568015399834976176, -3.295601554149325541 ) ) ;
#22868 = LINE ( 'NONE', #4908, #7118 ) ;
#22869 = LINE ( 'NONE', #9729, #15064 ) ;
#22870 = DIRECTION ( 'NONE',  ( 0.000000000000000000, 0.000000000000000000, -1.000000000000000000 ) ) ;
#22871 = ORIENTED_EDGE ( 'NONE', *, *, #753, .T. ) ;
#22872 = COLOUR_RGB ( '', 0.72549020, 0.75294118, 0.79215686) ;
#22873 = CARTESIAN_POINT ( 'NONE',  ( 27.50000000000000000, 7.500000000000002665, -33.66025403784446723 ) ) ;
#22874 = VERTEX_POINT ( 'NONE', #22776 ) ;
#22875 = CARTESIAN_POINT ( 'NONE',  ( -66.75000000109245946, 8.538419263543522320, 16.46158073645647235 ) ) ;
#22876 = CONTEXT_DEPENDENT_SHAPE_REPRESENTATION ( #10099, #15483 ) ;
#22877 = EDGE_LOOP ( 'NONE', ( #981, #10867, #13951, #11654, #19490, #19601 ) ) ;
#22878 = CARTESIAN_POINT ( 'NONE',  ( 1.489200000000000079, 8.279592079675421725E-16, 6.760799999999997034 ) ) ;
#22879 = VERTEX_POINT ( 'NONE', #13942 ) ;
#22880 = CIRCLE ( 'NONE', #1444, 11.00000000000000000 ) ;
#22881 = AXIS2_PLACEMENT_3D ( 'NONE', #8554, #19547, #8448 ) ;
#22882 = PRESENTATION_LAYER_ASSIGNMENT (  '', '', ( #10302 ) ) ;
#22883 = ORIENTED_EDGE ( 'NONE', *, *, #12915, .T. ) ;
#22884 = CARTESIAN_POINT ( 'NONE',  ( -2.445694354108818303, -2.445694354108820967, 11.81250000136560629 ) ) ;
#22885 = CARTESIAN_POINT ( 'NONE',  ( -1.656854249492380582, 4.000000000000000000, -0.7624999972688126793 ) ) ;
#22886 = PLANE ( 'NONE',  #8709 ) ;
#22887 = DIRECTION ( 'NONE',  ( -1.000000000000000000, -7.703719777548943412E-32, 0.000000000000000000 ) ) ;
#22888 = CIRCLE ( 'NONE', #22508, 6.000000000000022204 ) ;
#22889 = CARTESIAN_POINT ( 'NONE',  ( -71.05000000000001137, 7.499999999999995559, 16.03553390593273420 ) ) ;
#22890 = DIRECTION ( 'NONE',  ( -1.000000000000000000, 0.000000000000000000, 0.000000000000000000 ) ) ;
#22891 = CARTESIAN_POINT ( 'NONE',  ( 58.74768183416157541, 7.123453452023678523, 17.78030770151605822 ) ) ;
#22892 = CARTESIAN_POINT ( 'NONE',  ( 4.999999999999999112, 0.4999240074894452657, 8.734705317681628500 ) ) ;
#22893 =( BOUNDED_CURVE ( )  B_SPLINE_CURVE ( 2, ( #14293, #17989, #3249, #9026, #19891, #19996, #21677, #7346, #19767 ),
 .UNSPECIFIED., .F., .F. ) 
 B_SPLINE_CURVE_WITH_KNOTS ( ( 3, 2, 2, 2, 3 ),
 ( 0.6875000000000001110, 0.7031250000000000000, 0.7187500000000000000, 0.7343749999999998890, 0.7499999999999997780 ),
 .UNSPECIFIED. ) 
 CURVE ( )  GEOMETRIC_REPRESENTATION_ITEM ( )  RATIONAL_B_SPLINE_CURVE ( ( 0.9999999999999994449, 0.9238795325112872936, 1.000000000000000000, 0.9238795325112867385, 1.000000000000000000, 0.9238795325112867385, 1.000000000000000000, 0.9238795325112878487, 0.9999999999999988898 ) ) 
 REPRESENTATION_ITEM ( '' )  );
#22894 = VECTOR ( 'NONE', #19118, 1000.000000000000000 ) ;
#22895 = CARTESIAN_POINT ( 'NONE',  ( 6.353591512924457348E-16, -3.458734125000000770, -0.7624999986344024316 ) ) ;
#22896 = CARTESIAN_POINT ( 'NONE',  ( 71.59999999999999432, 11.76776695296636888, 16.76776695296636532 ) ) ;
#22897 = CARTESIAN_POINT ( 'NONE',  ( -3.999999999999999112, 0.000000000000000000, 12.12500000273119838 ) ) ;
#22898 = DIRECTION ( 'NONE',  ( -1.000000000000000000, -7.703719777548943412E-32, 0.000000000000000000 ) ) ;
#22899 = ORIENTED_EDGE ( 'NONE', *, *, #20765, .F. ) ;
#22900 = DIRECTION ( 'NONE',  ( 0.000000000000000000, 0.000000000000000000, -1.000000000000000000 ) ) ;
#22901 = ORIENTED_EDGE ( 'NONE', *, *, #23330, .T. ) ;
#22902 = CARTESIAN_POINT ( 'NONE',  ( 51.99768183416157541, 12.16943976678977535, 12.92679907967048614 ) ) ;
#22903 = FILL_AREA_STYLE_COLOUR ( '', #7977 ) ;
#22904 = CIRCLE ( 'NONE', #23678, 5.560781378645573980 ) ;
#22905 = CARTESIAN_POINT ( 'NONE',  ( -3.458734124999999882, -1.432654583217642275, 1.800000001365597235 ) ) ;
#22906 = VERTEX_POINT ( 'NONE', #19298 ) ;
#22907 = CARTESIAN_POINT ( 'NONE',  ( 4.000000000000000000, 4.898587196589412829E-16, -0.1999999999999987899 ) ) ;
#22908 = TOROIDAL_SURFACE ( 'NONE', #12621, 6.200000000000021494, 0.1999999999999996503 ) ;
#22909 = EDGE_CURVE ( 'NONE', #15108, #23499, #6624, .T. ) ;
#22910 = VERTEX_POINT ( 'NONE', #17526 ) ;
#22911 = CARTESIAN_POINT ( 'NONE',  ( 1.656854249492381470, 4.000000000000000000, 19.68750000000001066 ) ) ;
#22912 = VERTEX_POINT ( 'NONE', #3009 ) ;
#22913 = CARTESIAN_POINT ( 'NONE',  ( 56.00231816583843170, 12.07320092032949610, 12.83056023321021044 ) ) ;
#22914 = CARTESIAN_POINT ( 'NONE',  ( 4.999999999999999112, -9.314797388894900720, 1.239665997526853580 ) ) ;
#22915 = CARTESIAN_POINT ( 'NONE',  ( -68.05000000218494449, 7.499999999999995559, 13.96446609406725692 ) ) ;
#22916 = CIRCLE ( 'NONE', #12628, 4.000000000000002665 ) ;
#22917 = CARTESIAN_POINT ( 'NONE',  ( -3.458734125000000326, -1.432654583217642497, -1.949999998634404097 ) ) ;
#22918 = PLANE ( 'NONE',  #10688 ) ;
#22919 = CARTESIAN_POINT ( 'NONE',  ( 66.19999999999998863, 8.232233047033627571, 16.76776695296636532 ) ) ;
#22920 = CARTESIAN_POINT ( 'NONE',  ( -3.999999999999998224, -1.656854249492383246, 15.18750000273119660 ) ) ;
#22921 = VECTOR ( 'NONE', #16390, 1000.000000000000000 ) ;
#22922 = FACE_OUTER_BOUND ( 'NONE', #15259, .T. ) ;
#22923 = CARTESIAN_POINT ( 'NONE',  ( 69.05000000109247082, 7.933012699999995476, 14.99999999999999645 ) ) ;
#22924 = AXIS2_PLACEMENT_3D ( 'NONE', #3541, #9198, #19700 ) ;
#22925 = CARTESIAN_POINT ( 'NONE',  ( -4.197393957002303999, -7.773935952363655451E-14, -3.503767560748929810 ) ) ;
#22926 = CARTESIAN_POINT ( 'NONE',  ( 57.59606816583843880, 11.17458954617364242, 11.97181229448534800 ) ) ;
#22927 = CARTESIAN_POINT ( 'NONE',  ( 6.353591512924457348E-16, -3.458734125000000770, 0.2375000013655967357 ) ) ;
#22928 = CARTESIAN_POINT ( 'NONE',  ( 4.000000000000000000, -2.309401076758514915, -3.433295621305383349 ) ) ;
#22929 = CARTESIAN_POINT ( 'NONE',  ( 70.09999999999999432, 9.999999999999998224, 17.49999999999999645 ) ) ;
#22930 = CARTESIAN_POINT ( 'NONE',  ( -69.95000000109247651, 8.538419263543522320, 16.46158073645647235 ) ) ;
#22931 = EDGE_LOOP ( 'NONE', ( #4058, #10727, #5587 ) ) ;
#22932 = DIRECTION ( 'NONE',  ( -1.000000000000000000, 0.000000000000000000, 0.000000000000000000 ) ) ;
#22933 = CARTESIAN_POINT ( 'NONE',  ( -4.000000000000000888, 1.656854249492380582, -1.762499999999997957 ) ) ;
#22934 = ORIENTED_EDGE ( 'NONE', *, *, #484, .F. ) ;
#22935 = CARTESIAN_POINT ( 'NONE',  ( 4.000000000000001776, -1.656854249492379694, 15.56250000273119660 ) ) ;
#22936 = PRESENTATION_LAYER_ASSIGNMENT (  '', '', ( #6119 ) ) ;
#22937 = CARTESIAN_POINT ( 'NONE',  ( -4.000000000000000888, 1.656854249492380804, 2.362500002731187987 ) ) ;
#22938 = ORIENTED_EDGE ( 'NONE', *, *, #13669, .F. ) ;
#22939 = ORIENTED_EDGE ( 'NONE', *, *, #9236, .F. ) ;
#22940 = EDGE_CURVE ( 'NONE', #12921, #18952, #13587, .T. ) ;
#22941 = FACE_BOUND ( 'NONE', #2406, .T. ) ;
#22942 = ADVANCED_FACE ( 'NONE', ( #6386, #2889 ), #13704, .F. ) ;
#22943 = CARTESIAN_POINT ( 'NONE',  ( 4.999999999999999112, 0.000000000000000000, 0.000000000000000000 ) ) ;
#22944 = ORIENTED_EDGE ( 'NONE', *, *, #2470, .F. ) ;
#22945 = CARTESIAN_POINT ( 'NONE',  ( 4.175002511812151873, 2.208363329454889445, -3.469254087858244073 ) ) ;
#22946 = CIRCLE ( 'NONE', #6070, 4.000000000000001776 ) ;
#22947 = CIRCLE ( 'NONE', #6514, 2.649999999999999467 ) ;
#22948 = PRODUCT_DEFINITION_CONTEXT ( 'detailed design', #11642, 'design' ) ;
#22949 = EDGE_CURVE ( 'NONE', #2643, #3575, #16079, .T. ) ;
#22950 = CARTESIAN_POINT ( 'NONE',  ( 69.60000000109249640, 10.85617417291294551, 17.06698729999999742 ) ) ;
#22951 = AXIS2_PLACEMENT_3D ( 'NONE', #21088, #15854, #15508 ) ;
#22952 = CARTESIAN_POINT ( 'NONE',  ( 66.75000000109245946, 8.538419263543522320, 16.46158073645647235 ) ) ;
#22953 = ORIENTED_EDGE ( 'NONE', *, *, #12623, .F. ) ;
#22954 = DIRECTION ( 'NONE',  ( 0.000000000000000000, 0.3090169943749481174, -0.9510565162951533091 ) ) ;
#22955 = CARTESIAN_POINT ( 'NONE',  ( 56.06250000000000000, 5.999999999999996447, 15.00000000000001599 ) ) ;
#22956 = CARTESIAN_POINT ( 'NONE',  ( 3.458734125000000326, 1.432654583217640498, 3.300000001365598568 ) ) ;
#22957 = CARTESIAN_POINT ( 'NONE',  ( 1.432654583217641164, 3.458734125000000326, 18.12500000136560274 ) ) ;
#22958 = DIRECTION ( 'NONE',  ( 0.000000000000000000, 0.000000000000000000, 1.000000000000000000 ) ) ;
#22959 = CARTESIAN_POINT ( 'NONE',  ( 0.000000000000000000, -10.90201369670499965, 1.464956435139506352 ) ) ;
#22960 = ORIENTED_EDGE ( 'NONE', *, *, #14104, .F. ) ;
#22961 = LINE ( 'NONE', #9698, #17616 ) ;
#22962 = CARTESIAN_POINT ( 'NONE',  ( -3.999999999999999112, 0.000000000000000000, 12.00000000000001066 ) ) ;
#22963 = DIRECTION ( 'NONE',  ( 0.5000000000000013323, 0.000000000000000000, 0.8660254037844380415 ) ) ;
#22964 = CIRCLE ( 'NONE', #11131, 1.020000000000000018 ) ;
#22965 = VERTEX_POINT ( 'NONE', #10004 ) ;
#22966 = EDGE_CURVE ( 'NONE', #4847, #5505, #15748, .T. ) ;
#22967 = PLANE ( 'NONE',  #12977 ) ;
#22968 = FACE_OUTER_BOUND ( 'NONE', #16150, .T. ) ;
#22969 = PRESENTATION_LAYER_ASSIGNMENT (  '', '', ( #17639 ) ) ;
#22970 = EDGE_CURVE ( 'NONE', #5149, #15108, #4460, .T. ) ;
#22971 = CYLINDRICAL_SURFACE ( 'NONE', #6801, 4.000000000000001776 ) ;
#22972 = ORIENTED_EDGE ( 'NONE', *, *, #17089, .F. ) ;
#22973 = CARTESIAN_POINT ( 'NONE',  ( -4.000000000000000000, -2.309401076758512694, -3.433295621305382461 ) ) ;
#22974 = ORIENTED_EDGE ( 'NONE', *, *, #23226, .T. ) ;
#22975 = CARTESIAN_POINT ( 'NONE',  ( 71.20000000109246230, 10.85617417291294551, 17.06698730000000097 ) ) ;
#22976 = EDGE_CURVE ( 'NONE', #4822, #2990, #1210, .T. ) ;
#22977 = CARTESIAN_POINT ( 'NONE',  ( 71.25000000218494733, 7.499999999999995559, 13.96446609406725692 ) ) ;
#22978 = EDGE_CURVE ( 'NONE', #9522, #21072, #1524, .T. ) ;
#22979 = CARTESIAN_POINT ( 'NONE',  ( 9.920644283265380691E-16, 4.000000000000000000, 21.31370849898476649 ) ) ;
#22980 = CARTESIAN_POINT ( 'NONE',  ( -6.259644161404860030E-16, -4.618802153517027165, -3.433295621305388234 ) ) ;
#22981 = CARTESIAN_POINT ( 'NONE',  ( 66.15000000109247935, 8.538419263543524096, 13.53841926354352054 ) ) ;
#22982 = ORIENTED_EDGE ( 'NONE', *, *, #6055, .F. ) ;
#22983 = VECTOR ( 'NONE', #19860, 1000.000000000000114 ) ;
#22984 = DIRECTION ( 'NONE',  ( 1.000000000000000000, 0.000000000000000000, 0.000000000000000000 ) ) ;
#22985 = FACE_OUTER_BOUND ( 'NONE', #8265, .T. ) ;
#22986 = CARTESIAN_POINT ( 'NONE',  ( 71.00000000109245946, 9.143825827087050939, 12.93301269999999370 ) ) ;
#22987 = CARTESIAN_POINT ( 'NONE',  ( -1.432654583217638944, 3.458734125000000326, 10.25000000136560452 ) ) ;
#22988 = CARTESIAN_POINT ( 'NONE',  ( 7.829898480332751376, -11.25000000000000355, 5.000000000000079936 ) ) ;
#22989 = DIRECTION ( 'NONE',  ( 0.000000000000000000, 1.000000000000000000, 3.469446951953612611E-15 ) ) ;
#22990 = VERTEX_POINT ( 'NONE', #8437 ) ;
#22991 = CARTESIAN_POINT ( 'NONE',  ( -4.000000000000000888, 1.656854249492380804, -0.7624999999999970690 ) ) ;
#22992 = CARTESIAN_POINT ( 'NONE',  ( -2.828427124746189403, 2.828427124746190291, 15.87500000000001066 ) ) ;
#22993 = DIRECTION ( 'NONE',  ( -1.000000000000000000, 0.000000000000000000, 0.000000000000000000 ) ) ;
#22994 = CARTESIAN_POINT ( 'NONE',  ( -1.520000000000000462, 0.000000000000000000, -8.239200000000002078 ) ) ;
#22995 = EDGE_LOOP ( 'NONE', ( #15491, #11091, #22229, #6005, #9301, #1079 ) ) ;
#22996 = CARTESIAN_POINT ( 'NONE',  ( 4.000000000000001776, -1.656854249492379694, 13.56250000273119660 ) ) ;
#22997 = VERTEX_POINT ( 'NONE', #15628 ) ;
#22998 = CARTESIAN_POINT ( 'NONE',  ( -66.20000000109246230, 9.143825827087050939, 12.93301269999999370 ) ) ;
#22999 = ITEM_DEFINED_TRANSFORMATION ( 'NONE', 'NONE', #1486,  #7318 ) ;
#23000 = ADVANCED_FACE ( 'NONE', ( #11682 ), #19190, .T. ) ;
#23001 = VERTEX_POINT ( 'NONE', #751 ) ;
#23002 = DIRECTION ( 'NONE',  ( 0.000000000000000000, 0.000000000000000000, -1.000000000000000000 ) ) ;
#23003 = ORIENTED_EDGE ( 'NONE', *, *, #9496, .T. ) ;
#23004 =( BOUNDED_CURVE ( )  B_SPLINE_CURVE ( 2, ( #1267, #14358, #3191, #5352, #19950, #23554, #14120, #19711, #4876 ),
 .UNSPECIFIED., .F., .F. ) 
 B_SPLINE_CURVE_WITH_KNOTS ( ( 3, 2, 2, 2, 3 ),
 ( 0.6250000000000005551, 0.6406250000000004441, 0.6562500000000003331, 0.6718750000000002220, 0.6875000000000001110 ),
 .UNSPECIFIED. ) 
 CURVE ( )  GEOMETRIC_REPRESENTATION_ITEM ( )  RATIONAL_B_SPLINE_CURVE ( ( 0.9999999999999973355, 0.9238795325112894030, 1.000000000000000000, 0.9238795325112867385, 1.000000000000000000, 0.9238795325112867385, 1.000000000000000000, 0.9238795325112861834, 1.000000000000000444 ) ) 
 REPRESENTATION_ITEM ( '' )  );
#23005 = VERTEX_POINT ( 'NONE', #15396 ) ;
#23006 = CARTESIAN_POINT ( 'NONE',  ( 1.872352939448454495E-15, -3.458734125000000770, 13.93750000136560629 ) ) ;
#23007 = CARTESIAN_POINT ( 'NONE',  ( 51.00000000000000711, 12.12132034355963484, 12.87867965644034740 ) ) ;
#23008 = EDGE_CURVE ( 'NONE', #2702, #11449, #18951, .T. ) ;
#23009 = DIRECTION ( 'NONE',  ( -0.9396926207859107594, -0.3420201433256623291, 1.540743955509804830E-32 ) ) ;
#23010 = CARTESIAN_POINT ( 'NONE',  ( 66.50000000109247367, 9.143825827087049163, 17.06698730000000097 ) ) ;
#23011 = CARTESIAN_POINT ( 'NONE',  ( -69.70000000000000284, 9.999999999999998224, 12.49999999999999289 ) ) ;
#23012 = CARTESIAN_POINT ( 'NONE',  ( 6.500000000000000888, -2.517290933526017405, -0.2565799252183981749 ) ) ;
#23013 = CARTESIAN_POINT ( 'NONE',  ( 57.62268183416157541, 12.78030770151606177, 17.87654654797631792 ) ) ;
#23014 = CARTESIAN_POINT ( 'NONE',  ( 59.99999999999999289, 11.45040179400661096, 18.39307336842673735 ) ) ;
#23015 = CARTESIAN_POINT ( 'NONE',  ( 2.445694354108820079, 2.445694354108820523, 0.6125000013655953479 ) ) ;
#23016 = CARTESIAN_POINT ( 'NONE',  ( -3.999999999999999112, 0.000000000000000000, 21.31370849898476649 ) ) ;
#23017 = DIRECTION ( 'NONE',  ( -1.000000000000000000, -0.000000000000000000, -0.000000000000000000 ) ) ;
#23018 = CARTESIAN_POINT ( 'NONE',  ( -2.828427124746188515, -2.828427124746190735, 11.25000000273119660 ) ) ;
#23019 = CARTESIAN_POINT ( 'NONE',  ( -14.16125006966725053, -11.25000000000000355, 5.000000000000079936 ) ) ;
#23020 = ORIENTED_EDGE ( 'NONE', *, *, #14945, .F. ) ;
#23021 = CARTESIAN_POINT ( 'NONE',  ( 4.000000000000000888, 4.898587196589412829E-16, 16.62500000273119838 ) ) ;
#23022 = ORIENTED_EDGE ( 'NONE', *, *, #11603, .T. ) ;
#23023 = CARTESIAN_POINT ( 'NONE',  ( 55.18518183416157541, 10.06805114094562548, 11.99999999999999645 ) ) ;
#23024 = CARTESIAN_POINT ( 'NONE',  ( -69.35000000109248219, 11.46158073645647235, 13.53841926354352232 ) ) ;
#23025 = CARTESIAN_POINT ( 'NONE',  ( -6.500000000000000000, 3.752776749732564809, -3.700000000000000178 ) ) ;
#23026 = ORIENTED_EDGE ( 'NONE', *, *, #3169, .T. ) ;
#23027 = FACE_OUTER_BOUND ( 'NONE', #11487, .T. ) ;
#23028 = EDGE_LOOP ( 'NONE', ( #8991, #11960, #13069, #19416, #22646, #13152 ) ) ;
#23029 = FACE_OUTER_BOUND ( 'NONE', #16577, .T. ) ;
#23030 = ORIENTED_EDGE ( 'NONE', *, *, #4398, .F. ) ;
#23031 = EDGE_CURVE ( 'NONE', #10020, #19518, #8086, .T. ) ;
#23032 = CARTESIAN_POINT ( 'NONE',  ( 51.22106816583844591, 14.02818770551465377, 16.58880310854672757 ) ) ;
#23033 = CARTESIAN_POINT ( 'NONE',  ( -66.30000000218494449, 8.232233047033627571, 16.76776695296636532 ) ) ;
#23034 = CARTESIAN_POINT ( 'NONE',  ( 14.94766720513313096, 3.719910619709361654, 10.00000000000008882 ) ) ;
#23035 = FACE_OUTER_BOUND ( 'NONE', #3446, .T. ) ;
#23036 = CARTESIAN_POINT ( 'NONE',  ( 1.025207404391860050E-15, 3.458734125000000326, 10.18750000136560629 ) ) ;
#23037 = CARTESIAN_POINT ( 'NONE',  ( -1.656854249492380138, -3.999999999999999112, 14.31250000273119660 ) ) ;
#23038 = CARTESIAN_POINT ( 'NONE',  ( 57.46875000000000711, 6.999999999999992895, 13.75735931288071967 ) ) ;
#23039 = CARTESIAN_POINT ( 'NONE',  ( 68.40000000109249356, 9.143825827087050939, 12.93301269999999370 ) ) ;
#23040 = DIRECTION ( 'NONE',  ( 0.000000000000000000, 0.000000000000000000, -1.000000000000000000 ) ) ;
#23041 = CARTESIAN_POINT ( 'NONE',  ( 52.15856816583843880, 7.028187705514647554, 16.31069182806492179 ) ) ;
#23042 = CARTESIAN_POINT ( 'NONE',  ( -3.458734125000000326, -1.432654583217642497, 1.050000001365596791 ) ) ;
#23043 = CARTESIAN_POINT ( 'NONE',  ( -1.432654583217639832, -3.458734125000000326, 10.87500000136560452 ) ) ;
#23044 = CARTESIAN_POINT ( 'NONE',  ( 67.45000000000000284, 12.50000000000000000, 13.96446609406725692 ) ) ;
#23045 = CARTESIAN_POINT ( 'NONE',  ( -68.00000000109245946, 12.06698729999999919, 14.14382582708705094 ) ) ;
#23046 = VERTEX_POINT ( 'NONE', #22659 ) ;
#23047 = LINE ( 'NONE', #9053, #12019 ) ;
#23048 = CARTESIAN_POINT ( 'NONE',  ( -1.656854249492380582, 4.000000000000000000, -1.887499999999998179 ) ) ;
#23049 = EDGE_LOOP ( 'NONE', ( #23020, #4622, #8309, #20918 ) ) ;
#23050 = DIRECTION ( 'NONE',  ( 0.3420201433256622181, 0.9396926207859107594, -6.162975822039141593E-32 ) ) ;
#23051 = CARTESIAN_POINT ( 'NONE',  ( -2.828427124746190291, 2.828427124746190291, -0.6999999972688124572 ) ) ;
#23052 = EDGE_LOOP ( 'NONE', ( #15890, #1661, #19373, #22934 ) ) ;
#23053 = ORIENTED_EDGE ( 'NONE', *, *, #21516, .T. ) ;
#23054 = PLANE ( 'NONE',  #10258 ) ;
#23055 = DIRECTION ( 'NONE',  ( 0.000000000000000000, 0.000000000000000000, -1.000000000000000000 ) ) ;
#23056 = ORIENTED_EDGE ( 'NONE', *, *, #23156, .T. ) ;
#23057 = CARTESIAN_POINT ( 'NONE',  ( 0.5636800770130377947, 4.293361309317166530, -3.531542292954102713 ) ) ;
#23058 = CARTESIAN_POINT ( 'NONE',  ( 69.65000000109247935, 9.999999999999998224, 17.06698730000000097 ) ) ;
#23059 = CIRCLE ( 'NONE', #12395, 4.000000000000001776 ) ;
#23060 = CARTESIAN_POINT ( 'NONE',  ( 68.50000000109245946, 7.933012699999995476, 14.14382582708705094 ) ) ;
#23061 = VECTOR ( 'NONE', #18717, 1000.000000000000000 ) ;
#23062 = CARTESIAN_POINT ( 'NONE',  ( -1.656854249492380138, -3.999999999999999112, 17.31250000273119483 ) ) ;
#23063 = ADVANCED_FACE ( 'NONE', ( #860 ), #9878, .F. ) ;
#23064 = DIRECTION ( 'NONE',  ( 0.000000000000000000, -0.8660254037844390407, -0.4999999999999993339 ) ) ;
#23065 = CARTESIAN_POINT ( 'NONE',  ( 52.40625000000000000, 13.99999999999999289, 13.34314575050759544 ) ) ;
#23066 = CARTESIAN_POINT ( 'NONE',  ( 3.458734125000000326, 1.432654583217640498, 2.300000001365597679 ) ) ;
#23067 = CARTESIAN_POINT ( 'NONE',  ( 1.432654583217643163, -3.458734124999999437, 14.75000000136560452 ) ) ;
#23068 = FACE_OUTER_BOUND ( 'NONE', #18762, .T. ) ;
#23069 = DIRECTION ( 'NONE',  ( -0.9396926207859107594, -0.3420201433256623291, 1.540743955509804830E-32 ) ) ;
#23070 = VERTEX_POINT ( 'NONE', #12035 ) ;
#23071 = CARTESIAN_POINT ( 'NONE',  ( -3.556935580002248187, 0.06199486344584782122, 2.039999999999997371 ) ) ;
#23072 = CARTESIAN_POINT ( 'NONE',  ( -6.500000000000000000, 0.000000000000000000, -3.700000000000000178 ) ) ;
#23073 = DIRECTION ( 'NONE',  ( -1.000000000000000000, -0.000000000000000000, 0.000000000000000000 ) ) ;
#23074 = EDGE_CURVE ( 'NONE', #10244, #1974, #20272, .T. ) ;
#23075 = ORIENTED_EDGE ( 'NONE', *, *, #4507, .F. ) ;
#23076 = AXIS2_PLACEMENT_3D ( 'NONE', #2799, #15178, #6291 ) ;
#23077 = CARTESIAN_POINT ( 'NONE',  ( 37.82128094071656932, -8.974600000000002353, 10.00000000000008882 ) ) ;
#23078 = TOROIDAL_SURFACE ( 'NONE', #10106, 4.000000000000000000, 0.2500000000000000000 ) ;
#23079 = DIRECTION ( 'NONE',  ( 7.010384997569516610E-32, 1.000000000000000000, -3.469446951953615175E-16 ) ) ;
#23080 = VERTEX_POINT ( 'NONE', #2663 ) ;
#23081 = LINE ( 'NONE', #8382, #18700 ) ;
#23082 = ORIENTED_EDGE ( 'NONE', *, *, #2461, .T. ) ;
#23083 = CARTESIAN_POINT ( 'NONE',  ( 53.15625000000001421, 6.000000000000004441, 16.65685424949239390 ) ) ;
#23084 = CARTESIAN_POINT ( 'NONE',  ( 70.15000000218495302, 11.03553390593273598, 17.50000000000000355 ) ) ;
#23085 = CARTESIAN_POINT ( 'NONE',  ( 4.000000000000000888, 4.898587196589412829E-16, 16.50000000000001066 ) ) ;
#23086 = CARTESIAN_POINT ( 'NONE',  ( 1.656854249492381470, 4.000000000000000000, 11.68750000000001066 ) ) ;
#23087 = CARTESIAN_POINT ( 'NONE',  ( 68.00000000109245946, 12.06698729999999919, 14.14382582708705094 ) ) ;
#23088 = ORIENTED_EDGE ( 'NONE', *, *, #20329, .F. ) ;
#23089 = EDGE_CURVE ( 'NONE', #3670, #14717, #17408, .T. ) ;
#23090 = EDGE_CURVE ( 'NONE', #22668, #2142, #13832, .T. ) ;
#23091 = CARTESIAN_POINT ( 'NONE',  ( -1.656854249492381248, -3.999999999999999112, -1.387499997268811347 ) ) ;
#23092 = CARTESIAN_POINT ( 'NONE',  ( 66.75000000109245946, 8.538419263543522320, 16.46158073645647235 ) ) ;
#23093 = CARTESIAN_POINT ( 'NONE',  ( 2.445694354108822299, -2.445694354108820079, 19.06250000136560629 ) ) ;
#23094 = DIRECTION ( 'NONE',  ( -1.000000000000000000, -0.000000000000000000, -0.000000000000000000 ) ) ;
#23095 = CARTESIAN_POINT ( 'NONE',  ( 5.000000000000000888, 3.872983346207417021, 1.000000000000000000 ) ) ;
#23096 = ORIENTED_EDGE ( 'NONE', *, *, #6296, .F. ) ;
#23097 = CARTESIAN_POINT ( 'NONE',  ( -10.00000000000000000, 0.000000000000000000, 0.000000000000000000 ) ) ;
#23098 = DIRECTION ( 'NONE',  ( 0.000000000000000000, 0.4999999999999990008, -0.8660254037844391517 ) ) ;
#23099 = CARTESIAN_POINT ( 'NONE',  ( -2.500000000000000888, 0.000000000000000000, -4.974599999999998801 ) ) ;
#23100 = DIRECTION ( 'NONE',  ( -1.000000000000000000, -0.000000000000000000, -0.000000000000000000 ) ) ;
#23101 = EDGE_CURVE ( 'NONE', #2869, #4263, #17756, .T. ) ;
#23102 = ORIENTED_EDGE ( 'NONE', *, *, #7889, .F. ) ;
#23103 = CARTESIAN_POINT ( 'NONE',  ( -1.506022603841296270, 8.263794135966437014E-16, 6.735000000000022524 ) ) ;
#23104 = VERTEX_POINT ( 'NONE', #6853 ) ;
#23105 = CARTESIAN_POINT ( 'NONE',  ( -0.9413949561959078505, -0.3373062947069096484, -26.84672628368516811 ) ) ;
#23106 = ITEM_DEFINED_TRANSFORMATION ( 'NONE', 'NONE', #8029,  #7318 ) ;
#23107 = ORIENTED_EDGE ( 'NONE', *, *, #2061, .T. ) ;
#23108 = PLANE ( 'NONE',  #14402 ) ;
#23109 = VERTEX_POINT ( 'NONE', #10829 ) ;
#23110 = EDGE_LOOP ( 'NONE', ( #5620, #9609, #21416, #19195 ) ) ;
#23111 = CARTESIAN_POINT ( 'NONE',  ( 3.458734125000001658, 4.235727675282972223E-16, 11.18750000136560452 ) ) ;
#23112 = LINE ( 'NONE', #20841, #1157 ) ;
#23113 = DIRECTION ( 'NONE',  ( 1.000000000000000000, 7.703719777548943412E-32, 0.000000000000000000 ) ) ;
#23114 = EDGE_CURVE ( 'NONE', #8738, #10010, #9028, .T. ) ;
#23115 = CARTESIAN_POINT ( 'NONE',  ( 66.70000000109246230, 7.933012699999995476, 14.14382582708705094 ) ) ;
#23116 = VECTOR ( 'NONE', #7289, 1000.000000000000000 ) ;
#23117 = CIRCLE ( 'NONE', #5537, 4.000000000000001776 ) ;
#23118 = CARTESIAN_POINT ( 'NONE',  ( -69.39999999999999147, 8.232233047033627571, 16.76776695296636532 ) ) ;
#23119 = EDGE_CURVE ( 'NONE', #11906, #14307, #1800, .T. ) ;
#23120 = CARTESIAN_POINT ( 'NONE',  ( -2.000000000000007550, -3.464101615137749945, 0.000000000000000000 ) ) ;
#23121 = CARTESIAN_POINT ( 'NONE',  ( 60.00000000000004974, 13.87186598631677192, 14.01465949560290625 ) ) ;
#23122 = CARTESIAN_POINT ( 'NONE',  ( -2.445694354108820523, 2.445694354108820523, -1.137499998634402765 ) ) ;
#23123 = CARTESIAN_POINT ( 'NONE',  ( 4.000000000000000888, 4.898587196589412829E-16, 13.50000000000001066 ) ) ;
#23124 = CARTESIAN_POINT ( 'NONE',  ( 20.00000000000000355, -8.499999999999962697, 6.123233995736764507E-15 ) ) ;
#23125 = CARTESIAN_POINT ( 'NONE',  ( 1.432654583217643163, -3.458734124999999437, 16.75000000136560629 ) ) ;
#23126 = DIRECTION ( 'NONE',  ( 1.000000000000000000, 0.000000000000000000, -1.224646799147353207E-16 ) ) ;
#23127 = EDGE_CURVE ( 'NONE', #21471, #22617, #4991, .T. ) ;
#23128 = EDGE_CURVE ( 'NONE', #4526, #17446, #6144, .T. ) ;
#23129 = ORIENTED_EDGE ( 'NONE', *, *, #2736, .F. ) ;
#23130 = CARTESIAN_POINT ( 'NONE',  ( 4.000000000000000888, 4.898587196589412829E-16, 14.62500000273119660 ) ) ;
#23131 = ORIENTED_EDGE ( 'NONE', *, *, #9134, .F. ) ;
#23132 = CARTESIAN_POINT ( 'NONE',  ( 60.99768183416157541, 12.87654654797631792, 12.21969229848393113 ) ) ;
#23133 = CARTESIAN_POINT ( 'NONE',  ( -70.30000000109248504, 12.06698730000000275, 15.85617417291294196 ) ) ;
#23134 = SHAPE_REPRESENTATION_RELATIONSHIP ( 'NONE' , 'NONE' ,  #15757, #6193 ) ;
#23135 = CYLINDRICAL_SURFACE ( 'NONE', #12474, 2.500000000000002220 ) ;
#23136 = VERTEX_POINT ( 'NONE', #18104 ) ;
#23137 = CARTESIAN_POINT ( 'NONE',  ( -31.74999999999995737, 5.204748896376250699E-16, -4.250000000000000000 ) ) ;
#23138 = VECTOR ( 'NONE', #14391, 1000.000000000000000 ) ;
#23139 = ORIENTED_EDGE ( 'NONE', *, *, #1173, .F. ) ;
#23140 = VECTOR ( 'NONE', #537, 1000.000000000000000 ) ;
#23141 = LINE ( 'NONE', #12044, #4482 ) ;
#23142 = ORIENTED_EDGE ( 'NONE', *, *, #1306, .F. ) ;
#23143 = CARTESIAN_POINT ( 'NONE',  ( 51.12731816583844591, 12.87654654797634102, 17.78030770151602979 ) ) ;
#23144 = CARTESIAN_POINT ( 'NONE',  ( -66.80000000218494449, 12.50000000000000000, 14.99999999999999645 ) ) ;
#23145 = CARTESIAN_POINT ( 'NONE',  ( -27.50000000000000711, 1.500000000000003109, -36.31025403784446581 ) ) ;
#23146 = CARTESIAN_POINT ( 'NONE',  ( 3.254516946766198959, -9.000000000000003553, 5.000000000000079936 ) ) ;
#23147 = CARTESIAN_POINT ( 'NONE',  ( -1.432654583217639832, -3.458734125000000326, 15.87500000136560452 ) ) ;
#23148 = CARTESIAN_POINT ( 'NONE',  ( 65.00000000000000000, 15.00000000000000000, 10.00000000000007105 ) ) ;
#23149 = DIRECTION ( 'NONE',  ( 0.000000000000000000, 0.000000000000000000, 1.000000000000000000 ) ) ;
#23150 = CARTESIAN_POINT ( 'NONE',  ( 67.14999999999999147, 7.499999999999996447, 13.96446609406725514 ) ) ;
#23151 = AXIS2_PLACEMENT_3D ( 'NONE', #7734, #15050, #632 ) ;
#23152 = CARTESIAN_POINT ( 'NONE',  ( 57.18750000000000000, 9.999999999999989342, 11.99999999999999467 ) ) ;
#23153 = AXIS2_PLACEMENT_3D ( 'NONE', #18049, #14596, #3657 ) ;
#23154 = CARTESIAN_POINT ( 'NONE',  ( -2.445694354108819635, -2.445694354108820967, 0.1125000013655966247 ) ) ;
#23155 = CARTESIAN_POINT ( 'NONE',  ( -0.6665512827318446076, -3.401344631923079120, 2.039999999999997815 ) ) ;
#23156 = EDGE_CURVE ( 'NONE', #19783, #10249, #14048, .T. ) ;
#23157 = SURFACE_STYLE_FILL_AREA ( #2807 ) ;
#23158 = EDGE_CURVE ( 'NONE', #7520, #13999, #3251, .T. ) ;
#23159 = ORIENTED_EDGE ( 'NONE', *, *, #14173, .F. ) ;
#23160 = LINE ( 'NONE', #4971, #3323 ) ;
#23161 = CARTESIAN_POINT ( 'NONE',  ( 22.10407284676620066, -9.000000000000001776, 10.00000000000008882 ) ) ;
#23162 = ORIENTED_EDGE ( 'NONE', *, *, #21069, .F. ) ;
#23163 = DIRECTION ( 'NONE',  ( 1.000000000000000000, 0.000000000000000000, 0.000000000000000000 ) ) ;
#23164 = CARTESIAN_POINT ( 'NONE',  ( 7.347880794884118750E-16, -4.000000000000000000, -1.324999997268811347 ) ) ;
#23165 = VERTEX_POINT ( 'NONE', #18219 ) ;
#23166 = EDGE_LOOP ( 'NONE', ( #11087, #14604, #4827, #18166 ) ) ;
#23167 = AXIS2_PLACEMENT_3D ( 'NONE', #3081, #6925, #14242 ) ;
#23168 = PRESENTATION_STYLE_ASSIGNMENT (( #16239 ) ) ;
#23169 = CARTESIAN_POINT ( 'NONE',  ( -66.79999999999999716, 11.76776695296636888, 16.76776695296636532 ) ) ;
#23170 = ORIENTED_EDGE ( 'NONE', *, *, #16247, .F. ) ;
#23171 = DIRECTION ( 'NONE',  ( -0.000000000000000000, 1.000000000000000000, -0.000000000000000000 ) ) ;
#23172 = UNCERTAINTY_MEASURE_WITH_UNIT (LENGTH_MEASURE( 1.000000000000000082E-05 ), #4493, 'distance_accuracy_value', 'NONE');
#23173 = CARTESIAN_POINT ( 'NONE',  ( -69.40000000218495302, 9.999999999999998224, 17.49999999999999645 ) ) ;
#23174 = EDGE_LOOP ( 'NONE', ( #15863, #19112, #4973, #9101 ) ) ;
#23175 = CARTESIAN_POINT ( 'NONE',  ( -1.600000000000004086, 0.000000000000000000, 0.000000000000000000 ) ) ;
#23176 = CARTESIAN_POINT ( 'NONE',  ( 66.30000000109247082, 10.85617417291294551, 12.93301269999999370 ) ) ;
#23177 = FACE_OUTER_BOUND ( 'NONE', #20565, .T. ) ;
#23178 = DIRECTION ( 'NONE',  ( 0.000000000000000000, 0.000000000000000000, 1.000000000000000000 ) ) ;
#23179 = CARTESIAN_POINT ( 'NONE',  ( 55.72106816583844591, 14.02818770551465377, 16.58880310854672757 ) ) ;
#23180 = CARTESIAN_POINT ( 'NONE',  ( -3.458734124999999882, -1.432654583217642497, 4.800000001365595459 ) ) ;
#23181 = CARTESIAN_POINT ( 'NONE',  ( 1.432654583217641164, 3.458734125000000326, 13.12500000136560629 ) ) ;
#23182 = DIRECTION ( 'NONE',  ( 0.000000000000000000, 0.000000000000000000, 1.000000000000000000 ) ) ;
#23183 = CARTESIAN_POINT ( 'NONE',  ( 5.577176569667260608, -11.25000000000000355, 10.00000000000008882 ) ) ;
#23184 = ORIENTED_EDGE ( 'NONE', *, *, #17044, .T. ) ;
#23185 = CARTESIAN_POINT ( 'NONE',  ( -2.503920655715996979, 2.852548534406722069, 2.039999999999996927 ) ) ;
#23186 = FACE_OUTER_BOUND ( 'NONE', #12672, .T. ) ;
#23187 = LINE ( 'NONE', #8604, #10068 ) ;
#23188 = ORIENTED_EDGE ( 'NONE', *, *, #19014, .T. ) ;
#23189 = CARTESIAN_POINT ( 'NONE',  ( 14.11308378033275446, -11.25000000000000355, 5.000000000000079936 ) ) ;
#23190 = CARTESIAN_POINT ( 'NONE',  ( -67.29999999999999716, 9.999999999999998224, 12.49999999999999289 ) ) ;
#23191 = CARTESIAN_POINT ( 'NONE',  ( 10.14331325928345073, -8.974600000000002353, 5.000000000000079936 ) ) ;
#23192 = ORIENTED_EDGE ( 'NONE', *, *, #2371, .F. ) ;
#23193 = CARTESIAN_POINT ( 'NONE',  ( -69.45000000000000284, 7.499999999999996447, 16.03553390593273775 ) ) ;
#23194 = ORIENTED_EDGE ( 'NONE', *, *, #16738, .T. ) ;
#23195 = EDGE_CURVE ( 'NONE', #7989, #9313, #22454, .T. ) ;
#23196 = CARTESIAN_POINT ( 'NONE',  ( 58.06481816583843170, 5.999999999999996447, 15.06805114094564502 ) ) ;
#23197 = CARTESIAN_POINT ( 'NONE',  ( 67.50000000218494733, 11.76776695296636888, 13.23223304703362579 ) ) ;
#23198 = AXIS2_PLACEMENT_3D ( 'NONE', #1479, #17675, #4845 ) ;
#23199 = DIRECTION ( 'NONE',  ( 0.000000000000000000, 0.000000000000000000, -1.000000000000000000 ) ) ;
#23200 = DIRECTION ( 'NONE',  ( 1.000000000000000000, 0.000000000000000000, -0.000000000000000000 ) ) ;
#23201 = CARTESIAN_POINT ( 'NONE',  ( 67.80000000109247082, 9.143825827087052716, 12.93301269999999192 ) ) ;
#23202 = ORIENTED_EDGE ( 'NONE', *, *, #8530, .T. ) ;
#23203 = CARTESIAN_POINT ( 'NONE',  ( 0.000000000000000000, 2.223716399045689407, -8.461683424509292450 ) ) ;
#23204 = FACE_OUTER_BOUND ( 'NONE', #11421, .T. ) ;
#23205 = CARTESIAN_POINT ( 'NONE',  ( 65.95000000109246230, 8.538419263543522320, 16.46158073645647235 ) ) ;
#23206 = CIRCLE ( 'NONE', #17545, 2.649999999999999467 ) ;
#23207 = CARTESIAN_POINT ( 'NONE',  ( 1.025207404391860050E-15, 3.458734125000000770, 19.43750000136560629 ) ) ;
#23208 = DIRECTION ( 'NONE',  ( 0.3420201433256622181, 0.9396926207859107594, -6.162975822039141593E-32 ) ) ;
#23209 = VECTOR ( 'NONE', #15867, 1000.000000000000000 ) ;
#23210 = DIRECTION ( 'NONE',  ( -1.000000000000000000, -0.000000000000000000, -0.000000000000000000 ) ) ;
#23211 = ORIENTED_EDGE ( 'NONE', *, *, #846, .T. ) ;
#23212 = CARTESIAN_POINT ( 'NONE',  ( -3.250000000000004441, 5.629165124598849879, 0.000000000000000000 ) ) ;
#23213 = CARTESIAN_POINT ( 'NONE',  ( 59.43750000000000711, 10.00000000000000711, 17.99999999999999645 ) ) ;
#23214 = DIRECTION ( 'NONE',  ( 0.000000000000000000, 0.000000000000000000, -1.000000000000000000 ) ) ;
#23215 = FILL_AREA_STYLE_COLOUR ( '', #13822 ) ;
#23216 = VERTEX_POINT ( 'NONE', #8782 ) ;
#23217 = DIRECTION ( 'NONE',  ( 0.000000000000000000, 0.000000000000000000, 1.000000000000000000 ) ) ;
#23218 = CARTESIAN_POINT ( 'NONE',  ( -2.445694354108820523, 2.445694354108820523, -0.3874999986344038194 ) ) ;
#23219 = CARTESIAN_POINT ( 'NONE',  ( 2.171643655288379993, -3.365003104552334978, -1.195831703456429434E-14 ) ) ;
#23220 = ORIENTED_EDGE ( 'NONE', *, *, #12946, .T. ) ;
#23221 = DIRECTION ( 'NONE',  ( 1.000000000000000000, -0.000000000000000000, -0.000000000000000000 ) ) ;
#23222 = EDGE_LOOP ( 'NONE', ( #115, #18004, #3385, #867 ) ) ;
#23223 = AXIS2_PLACEMENT_3D ( 'NONE', #18554, #6227, #9834 ) ;
#23224 = EDGE_CURVE ( 'NONE', #18376, #19953, #8679, .T. ) ;
#23225 = CARTESIAN_POINT ( 'NONE',  ( 4.000000000000000000, -2.309401076758516691, -0.4999999999999995559 ) ) ;
#23226 = EDGE_CURVE ( 'NONE', #19389, #7167, #10475, .T. ) ;
#23227 = EDGE_LOOP ( 'NONE', ( #7412, #17528, #4213, #14267 ) ) ;
#23228 = CARTESIAN_POINT ( 'NONE',  ( -2.445694354108819191, 2.445694354108820523, 14.56250000136560452 ) ) ;
#23229 = DIRECTION ( 'NONE',  ( -1.000000000000000000, 0.000000000000000000, -0.000000000000000000 ) ) ;
#23230 = CIRCLE ( 'NONE', #20546, 0.03079999999999923077 ) ;
#23231 = CARTESIAN_POINT ( 'NONE',  ( -66.85000000218495586, 12.50000000000000000, 16.03553390593273775 ) ) ;
#23232 = CARTESIAN_POINT ( 'NONE',  ( 67.45000000109246230, 7.933012699999995476, 14.99999999999999645 ) ) ;
#23233 = EDGE_CURVE ( 'NONE', #9734, #5914, #23373, .T. ) ;
#23234 = DIRECTION ( 'NONE',  ( -0.000000000000000000, -1.000000000000000000, -0.000000000000000000 ) ) ;
#23235 = CARTESIAN_POINT ( 'NONE',  ( -70.89999999999999147, 9.999999999999998224, 17.49999999999999645 ) ) ;
#23236 = DIRECTION ( 'NONE',  ( -1.000000000000000000, -7.703719777548943412E-32, 0.000000000000000000 ) ) ;
#23237 = CARTESIAN_POINT ( 'NONE',  ( 60.00000000000000711, 10.89310377415101350, 18.37602675929336016 ) ) ;
#23238 = VECTOR ( 'NONE', #21541, 1000.000000000000000 ) ;
#23239 = CARTESIAN_POINT ( 'NONE',  ( -3.458734125000000326, -1.432654583217642497, -1.949999998634404319 ) ) ;
#23240 = CARTESIAN_POINT ( 'NONE',  ( -67.80000000218494449, 9.999999999999998224, 17.49999999999999645 ) ) ;
#23241 = DIRECTION ( 'NONE',  ( 0.000000000000000000, 0.000000000000000000, -1.000000000000000000 ) ) ;
#23242 = CARTESIAN_POINT ( 'NONE',  ( 3.458734125000001214, 4.235727675282971730E-16, 16.93750000136560629 ) ) ;
#23243 = CARTESIAN_POINT ( 'NONE',  ( 4.197393957002303999, 7.772902908466098641E-14, -3.503767560748929810 ) ) ;
#23244 = VECTOR ( 'NONE', #637, 1000.000000000000000 ) ;
#23245 = VERTEX_POINT ( 'NONE', #15962 ) ;
#23246 = AXIS2_PLACEMENT_3D ( 'NONE', #15756, #13714, #14190 ) ;
#23247 = LINE ( 'NONE', #19895, #18521 ) ;
#23248 = ORIENTED_EDGE ( 'NONE', *, *, #9360, .F. ) ;
#23249 = CARTESIAN_POINT ( 'NONE',  ( 55.09143183416158962, 11.31069182806491291, 12.02818770551463778 ) ) ;
#23250 = CARTESIAN_POINT ( 'NONE',  ( -68.75000000109247367, 11.46158073645647235, 16.46158073645647235 ) ) ;
#23251 = DIRECTION ( 'NONE',  ( 1.118373553621255183E-32, -0.9073324201775119224, 0.4204139380358593581 ) ) ;
#23252 =( GEOMETRIC_REPRESENTATION_CONTEXT ( 3 ) GLOBAL_UNCERTAINTY_ASSIGNED_CONTEXT ( ( #2580 ) ) GLOBAL_UNIT_ASSIGNED_CONTEXT ( ( #9292, #12417, #16581 ) ) REPRESENTATION_CONTEXT ( 'NONE', 'WORKASPACE' ) );
#23253 = ADVANCED_FACE ( 'NONE', ( #12633 ), #5364, .F. ) ;
#23254 = LINE ( 'NONE', #1216, #21224 ) ;
#23255 = ORIENTED_EDGE ( 'NONE', *, *, #12450, .F. ) ;
#23256 = CARTESIAN_POINT ( 'NONE',  ( -15.00000000000001066, 10.00000000000000000, -49.99999999999999289 ) ) ;
#23257 = EDGE_CURVE ( 'NONE', #16922, #14633, #14178, .T. ) ;
#23258 = ADVANCED_FACE ( 'NONE', ( #21438 ), #5052, .T. ) ;
#23259 = ORIENTED_EDGE ( 'NONE', *, *, #10697, .T. ) ;
#23260 = CARTESIAN_POINT ( 'NONE',  ( 47.24605889071655440, -8.974600000000002353, 5.000000000000079936 ) ) ;
#23261 = ORIENTED_EDGE ( 'NONE', *, *, #5657, .F. ) ;
#23262 = CARTESIAN_POINT ( 'NONE',  ( 58.90856816583844591, 12.97181229448534978, 13.68930817193506755 ) ) ;
#23263 = VECTOR ( 'NONE', #20217, 1000.000000000000000 ) ;
#23264 = CARTESIAN_POINT ( 'NONE',  ( -68.30000000218494449, 11.76776695296636888, 13.23223304703362579 ) ) ;
#23265 = ADVANCED_FACE ( 'NONE', ( #14295 ), #12510, .T. ) ;
#23266 = CARTESIAN_POINT ( 'NONE',  ( 5.200000000000002842, 3.061616997868383634E-16, -2.500000000000000444 ) ) ;
#23267 = EDGE_CURVE ( 'NONE', #4326, #3825, #14772, .T. ) ;
#23268 = AXIS2_PLACEMENT_3D ( 'NONE', #8145, #19012, #19487 ) ;
#23269 = CARTESIAN_POINT ( 'NONE',  ( -19.99999999999999645, -11.25000000000000355, 5.000000000000079936 ) ) ;
#23270 = AXIS2_PLACEMENT_3D ( 'NONE', #14999, #20453, #13188 ) ;
#23271 = CARTESIAN_POINT ( 'NONE',  ( 3.458734125000002546, -1.432654583217639610, 15.12500000136560807 ) ) ;
#23272 = CARTESIAN_POINT ( 'NONE',  ( 1.656854249492383024, -3.999999999999999112, -2.262499997268812013 ) ) ;
#23273 = CARTESIAN_POINT ( 'NONE',  ( 57.00000000000000000, 12.12132034355963484, 12.87867965644034740 ) ) ;
#23274 = CARTESIAN_POINT ( 'NONE',  ( -65.00000000000000000, -10.00000000000000178, 17.49999999999999645 ) ) ;
#23275 = CARTESIAN_POINT ( 'NONE',  ( 58.03125000000000711, 11.24264068711929276, 18.00000000000000355 ) ) ;
#23276 = CARTESIAN_POINT ( 'NONE',  ( -2.445694354108819635, -2.445694354108820967, 1.112500001365595681 ) ) ;
#23277 = DIRECTION ( 'NONE',  ( -1.000000000000000000, -0.000000000000000000, -0.000000000000000000 ) ) ;
#23278 = CIRCLE ( 'NONE', #6089, 0.1999999999999996503 ) ;
#23279 = CARTESIAN_POINT ( 'NONE',  ( 70.20000000218495018, 9.999999999999998224, 17.49999999999999645 ) ) ;
#23280 = AXIS2_PLACEMENT_3D ( 'NONE', #7851, #9899, #4477 ) ;
#23281 = ORIENTED_EDGE ( 'NONE', *, *, #784, .T. ) ;
#23282 = LINE ( 'NONE', #6769, #11395 ) ;
#23283 = DIRECTION ( 'NONE',  ( -1.000000000000000000, 0.000000000000000000, 0.000000000000000000 ) ) ;
#23284 = ORIENTED_EDGE ( 'NONE', *, *, #10165, .F. ) ;
#23285 = LINE ( 'NONE', #8344, #11534 ) ;
#23286 = CARTESIAN_POINT ( 'NONE',  ( 4.000000000000000000, 1.656854249492381248, 0.9875000027311869877 ) ) ;
#23287 = PLANE ( 'NONE',  #22363 ) ;
#23288 = VERTEX_POINT ( 'NONE', #4203 ) ;
#23289 = VERTEX_POINT ( 'NONE', #9487 ) ;
#23290 = LINE ( 'NONE', #18142, #19794 ) ;
#23291 = AXIS2_PLACEMENT_3D ( 'NONE', #19231, #23171, #17686 ) ;
#23292 = EDGE_CURVE ( 'NONE', #20947, #7262, #18373, .T. ) ;
#23293 = DIRECTION ( 'NONE',  ( 1.000000000000000000, 0.000000000000000000, 0.000000000000000000 ) ) ;
#23294 = ORIENTED_EDGE ( 'NONE', *, *, #16422, .F. ) ;
#23295 = FACE_OUTER_BOUND ( 'NONE', #1418, .T. ) ;
#23296 = CIRCLE ( 'NONE', #15294, 1.000000000000002665 ) ;
#23297 = CARTESIAN_POINT ( 'NONE',  ( 1.656854249492384135, -3.999999999999999112, 11.31250000000001066 ) ) ;
#23298 = EDGE_CURVE ( 'NONE', #23527, #22848, #18814, .T. ) ;
#23299 = ORIENTED_EDGE ( 'NONE', *, *, #22047, .T. ) ;
#23300 = CIRCLE ( 'NONE', #14923, 8.749000000000004107 ) ;
#23301 = CARTESIAN_POINT ( 'NONE',  ( 66.15000000109247935, 11.46158073645647235, 13.53841926354352232 ) ) ;
#23302 = ADVANCED_FACE ( 'NONE', ( #7574 ), #2398, .F. ) ;
#23303 = VECTOR ( 'NONE', #13904, 1000.000000000000000 ) ;
#23304 = CARTESIAN_POINT ( 'NONE',  ( 71.34999999999999432, 11.03553390593273598, 12.49999999999999289 ) ) ;
#23305 = CARTESIAN_POINT ( 'NONE',  ( 0.000000000000000000, 0.000000000000000000, 0.000000000000000000 ) ) ;
#23306 = DIRECTION ( 'NONE',  ( 0.000000000000000000, 0.000000000000000000, -1.000000000000000000 ) ) ;
#23307 = CARTESIAN_POINT ( 'NONE',  ( 4.999999999999999112, -4.729683950898921907, 7.360373001730902587 ) ) ;
#23308 = CARTESIAN_POINT ( 'NONE',  ( 51.18750000000000711, 9.999999999999978684, 10.99999999999999645 ) ) ;
#23309 = CARTESIAN_POINT ( 'NONE',  ( -3.458734125000000326, 1.432654583217640276, 5.675000001365596347 ) ) ;
#23310 = CARTESIAN_POINT ( 'NONE',  ( -3.999999999999999112, 0.000000000000000000, 13.12500000273119660 ) ) ;
#23311 = CARTESIAN_POINT ( 'NONE',  ( -2.445694354108819191, 2.445694354108820523, 14.31250000136560452 ) ) ;
#23312 = CARTESIAN_POINT ( 'NONE',  ( -20.00005080000000035, 0.000000000000000000, 0.000000000000000000 ) ) ;
#23313 = CARTESIAN_POINT ( 'NONE',  ( 1.236993788156008760E-15, 0.000000000000000000, 21.31370849898476649 ) ) ;
#23314 = ORIENTED_EDGE ( 'NONE', *, *, #4661, .F. ) ;
#23315 = CARTESIAN_POINT ( 'NONE',  ( -0.9451720798219458430, 3.813322425661201276, 2.039999999999999147 ) ) ;
#23316 = ADVANCED_BREP_SHAPE_REPRESENTATION ( '', ( #14766, #7318 ), #21725 ) ;
#23317 = FACE_OUTER_BOUND ( 'NONE', #5356, .T. ) ;
#23318 = CARTESIAN_POINT ( 'NONE',  ( 13.28490590928345405, -8.974600000000002353, 5.000000000000079936 ) ) ;
#23319 = CIRCLE ( 'NONE', #19115, 8.265000000000021885 ) ;
#23320 = ORIENTED_EDGE ( 'NONE', *, *, #23397, .T. ) ;
#23321 = DIRECTION ( 'NONE',  ( 1.000000000000000000, 0.000000000000000000, 0.000000000000000000 ) ) ;
#23322 = CARTESIAN_POINT ( 'NONE',  ( -65.00000000000000000, -15.00000000000000000, 10.00000000000008882 ) ) ;
#23323 = CARTESIAN_POINT ( 'NONE',  ( 59.15625000000001421, 6.000000000000004441, 16.65685424949239390 ) ) ;
#23324 = EDGE_LOOP ( 'NONE', ( #8730, #1493, #8352 ) ) ;
#23325 = CARTESIAN_POINT ( 'NONE',  ( -69.29999999999999716, 9.999999999999998224, 17.49999999999999645 ) ) ;
#23326 = ORIENTED_EDGE ( 'NONE', *, *, #15106, .F. ) ;
#23327 = VECTOR ( 'NONE', #14475, 1000.000000000000000 ) ;
#23328 = CARTESIAN_POINT ( 'NONE',  ( 52.40625000000000000, 13.99999999999999289, 13.34314575050759544 ) ) ;
#23329 = AXIS2_PLACEMENT_3D ( 'NONE', #16435, #11056, #4080 ) ;
#23330 = EDGE_CURVE ( 'NONE', #13955, #19202, #18343, .T. ) ;
#23331 = CARTESIAN_POINT ( 'NONE',  ( 67.00000000218494733, 9.999999999999998224, 17.49999999999999645 ) ) ;
#23332 = CARTESIAN_POINT ( 'NONE',  ( -3.999999999999999112, 0.000000000000000000, 16.00000000000001066 ) ) ;
#23333 = LINE ( 'NONE', #84, #2963 ) ;
#23334 = DIRECTION ( 'NONE',  ( 0.3420201433256622736, -0.9396926207859106484, -1.232595164407828100E-31 ) ) ;
#23335 = ORIENTED_EDGE ( 'NONE', *, *, #12329, .T. ) ;
#23336 = AXIS2_PLACEMENT_3D ( 'NONE', #22042, #3864, #11199 ) ;
#23337 = CARTESIAN_POINT ( 'NONE',  ( 0.000000000000000000, 0.000000000000000000, -3.700000000000000178 ) ) ;
#23338 = LINE ( 'NONE', #1286, #18706 ) ;
#23339 = LINE ( 'NONE', #19857, #21364 ) ;
#23340 = CARTESIAN_POINT ( 'NONE',  ( 2.445694354108821411, 2.445694354108820523, 18.31250000136560274 ) ) ;
#23341 = CIRCLE ( 'NONE', #3461, 8.800000000000022027 ) ;
#23342 = DIRECTION ( 'NONE',  ( 0.000000000000000000, 0.000000000000000000, 1.000000000000000000 ) ) ;
#23343 = CARTESIAN_POINT ( 'NONE',  ( -2.762848947613220307, 4.746226468750993632, 10.00000000000000888 ) ) ;
#23344 = CIRCLE ( 'NONE', #7692, 11.00000000000000000 ) ;
#23345 = EDGE_LOOP ( 'NONE', ( #12493, #5087, #16995, #14579, #6978, #11969, #3354, #20394, #17562, #496, #15808, #22606, #7067, #15454, #2040, #10098, #12309, #14658, #22974, #17757, #3883, #14551, #5381, #1364, #12349, #23053, #19056, #15102, #16706, #5895, #13895, #13181, #18457, #11609, #21566, #9476, #7046, #17737, #19592, #8724, #11331, #5847, #3668, #3637, #13520, #4917, #1124, #6209, #20542, #8856, #7607, #5831, #7383, #9688, #21420, #11456, #5001, #14259, #104, #29, #11030, #6034, #10159, #6156, #19144, #19425, #7728, #19539, #4053, #8383, #19635, #201, #20479, #17661, #20505, #14425, #13043, #4775, #21973, #12247, #4060, #12388, #627, #6923, #14570, #19546, #7235, #19230, #11891, #3823, #10162, #2814, #20814 ) ) ;
#23346 = CARTESIAN_POINT ( 'NONE',  ( 1.656854249492383024, -3.999999999999999112, -1.387499999999997513 ) ) ;
#23347 = CARTESIAN_POINT ( 'NONE',  ( 56.62500000000000000, 12.12132034355964727, 17.12132034355963484 ) ) ;
#23348 = CARTESIAN_POINT ( 'NONE',  ( 66.79999999999999716, 11.76776695296636888, 16.76776695296636532 ) ) ;
#23349 = PRESENTATION_STYLE_ASSIGNMENT (( #16058 ) ) ;
#23350 = ORIENTED_EDGE ( 'NONE', *, *, #10697, .F. ) ;
#23351 = FACE_OUTER_BOUND ( 'NONE', #5439, .T. ) ;
#23352 = CARTESIAN_POINT ( 'NONE',  ( -2.445694354108820523, 2.445694354108820523, -1.387499998634402987 ) ) ;
#23353 = LINE ( 'NONE', #12249, #21959 ) ;
#23354 =( BOUNDED_CURVE ( )  B_SPLINE_CURVE ( 2, ( #20269, #5796, #16695, #7730, #22053, #13124, #21837, #1829, #2187 ),
 .UNSPECIFIED., .F., .F. ) 
 B_SPLINE_CURVE_WITH_KNOTS ( ( 3, 2, 2, 2, 3 ),
 ( 0.3125000000000002776, 0.3281250000000001665, 0.3437500000000001110, 0.3593750000000000000, 0.3749999999999998890 ),
 .UNSPECIFIED. ) 
 CURVE ( )  GEOMETRIC_REPRESENTATION_ITEM ( )  RATIONAL_B_SPLINE_CURVE ( ( 0.9999999999999986677, 0.9238795325112880708, 1.000000000000000000, 0.9238795325112867385, 1.000000000000000000, 0.9238795325112867385, 1.000000000000000000, 0.9238795325112872936, 0.9999999999999994449 ) ) 
 REPRESENTATION_ITEM ( '' )  );
#23355 = VERTEX_POINT ( 'NONE', #17 ) ;
#23356 = CARTESIAN_POINT ( 'NONE',  ( 4.999999999999999112, 0.000000000000000000, 0.000000000000000000 ) ) ;
#23357 = EDGE_LOOP ( 'NONE', ( #20927, #9318, #5420, #17571 ) ) ;
#23358 = CARTESIAN_POINT ( 'NONE',  ( -6.500000000000000000, 3.752776749732564809, -0.5805565836007661185 ) ) ;
#23359 = ORIENTED_EDGE ( 'NONE', *, *, #14816, .T. ) ;
#23360 = CARTESIAN_POINT ( 'NONE',  ( 1.971781867644420635E-15, -4.000000000000000000, 17.25000000000001066 ) ) ;
#23361 = CARTESIAN_POINT ( 'NONE',  ( 4.999999999999999112, 0.000000000000000000, 0.000000000000000000 ) ) ;
#23362 = AXIS2_PLACEMENT_3D ( 'NONE', #15125, #19798, #10745 ) ;
#23363 = DIRECTION ( 'NONE',  ( -1.000000000000000000, 0.000000000000000000, 0.000000000000000000 ) ) ;
#23364 = CARTESIAN_POINT ( 'NONE',  ( 0.9413949561959078505, 0.3373062947069096484, -26.84672628368516811 ) ) ;
#23365 = CARTESIAN_POINT ( 'NONE',  ( -13.27237933033274153, -11.25000000000000355, 10.00000000000008882 ) ) ;
#23366 = CARTESIAN_POINT ( 'NONE',  ( -71.24999999999998579, 8.964466094067258695, 12.49999999999999289 ) ) ;
#23367 = LINE ( 'NONE', #6971, #770 ) ;
#23368 = CARTESIAN_POINT ( 'NONE',  ( 60.00000000000000000, 13.47525482677739284, 13.02150377394223391 ) ) ;
#23369 = ADVANCED_FACE ( 'NONE', ( #20112 ), #18692, .T. ) ;
#23370 = CARTESIAN_POINT ( 'NONE',  ( 6.353591512924457348E-16, -3.458734125000000770, 1.237500001365595903 ) ) ;
#23371 = PLANE ( 'NONE',  #6911 ) ;
#23372 = CARTESIAN_POINT ( 'NONE',  ( -1.432654583217639610, -3.458734124999999882, 18.62500000136560274 ) ) ;
#23373 = LINE ( 'NONE', #14542, #17244 ) ;
#23374 = CIRCLE ( 'NONE', #5788, 11.00000000000000000 ) ;
#23375 = ORIENTED_EDGE ( 'NONE', *, *, #8101, .T. ) ;
#23376 = CARTESIAN_POINT ( 'NONE',  ( -70.85000000109246798, 9.999999999999998224, 12.93301269999999192 ) ) ;
#23377 = ORIENTED_EDGE ( 'NONE', *, *, #2334, .F. ) ;
#23378 = CARTESIAN_POINT ( 'NONE',  ( 52.84143183416158251, 8.689308171935088865, 17.97181229448535689 ) ) ;
#23379 = CARTESIAN_POINT ( 'NONE',  ( -68.20000000109246230, 7.933012699999995476, 15.85617417291294196 ) ) ;
#23380 = DIRECTION ( 'NONE',  ( 6.123233995736766036E-17, 1.000000000000000000, 0.000000000000000000 ) ) ;
#23381 = ADVANCED_FACE ( 'NONE', ( #11545 ), #7348, .T. ) ;
#23382 = CARTESIAN_POINT ( 'NONE',  ( -2.117863837641485618E-16, 3.458734125000000326, -2.512499998634404097 ) ) ;
#23383 = ORIENTED_EDGE ( 'NONE', *, *, #22727, .T. ) ;
#23384 = FACE_OUTER_BOUND ( 'NONE', #23222, .T. ) ;
#23385 = EDGE_LOOP ( 'NONE', ( #4734, #7735, #5593, #14752 ) ) ;
#23386 = CARTESIAN_POINT ( 'NONE',  ( -1.519999999999999574, 8.279592079675421725E-16, 6.760799999999997034 ) ) ;
#23387 = EDGE_LOOP ( 'NONE', ( #9218, #22220 ) ) ;
#23388 = CARTESIAN_POINT ( 'NONE',  ( 50.47106816583844591, 6.971812294485350670, 13.82541045382635403 ) ) ;
#23389 = CARTESIAN_POINT ( 'NONE',  ( -66.75000000218494733, 12.50000000000000000, 13.96446609406725869 ) ) ;
#23390 = DIRECTION ( 'NONE',  ( -0.000000000000000000, -1.000000000000000000, -0.000000000000000000 ) ) ;
#23391 = PLANE ( 'NONE',  #6072 ) ;
#23392 = CARTESIAN_POINT ( 'NONE',  ( -3.458734124999999437, 1.432654583217640498, 15.62500000136560629 ) ) ;
#23393 = CARTESIAN_POINT ( 'NONE',  ( -2.828427124746189403, 2.828427124746190291, 10.00000000273119660 ) ) ;
#23394 = CARTESIAN_POINT ( 'NONE',  ( 59.43750000000000711, 10.00000000000000711, 17.99999999999999645 ) ) ;
#23395 = EDGE_CURVE ( 'NONE', #19018, #5128, #19122, .T. ) ;
#23396 = CARTESIAN_POINT ( 'NONE',  ( 51.31481816583844591, 12.99999999999999822, 14.93194885905435676 ) ) ;
#23397 = EDGE_CURVE ( 'NONE', #12130, #10244, #4222, .T. ) ;
#23398 = CARTESIAN_POINT ( 'NONE',  ( -2.445694354108820523, 2.445694354108820523, -3.137499998634402765 ) ) ;
#23399 = FACE_OUTER_BOUND ( 'NONE', #1614, .T. ) ;
#23400 = CARTESIAN_POINT ( 'NONE',  ( 70.55000000218494449, 8.964466094067205404, 12.50000000000004263 ) ) ;
#23401 = ORIENTED_EDGE ( 'NONE', *, *, #615, .F. ) ;
#23402 = LINE ( 'NONE', #3159, #21269 ) ;
#23403 = CARTESIAN_POINT ( 'NONE',  ( -2.836893136758495970, -3.208949435745868328, -3.505054077164885484 ) ) ;
#23404 = VERTEX_POINT ( 'NONE', #13097 ) ;
#23405 = DIRECTION ( 'NONE',  ( 0.000000000000000000, 0.000000000000000000, -1.000000000000000000 ) ) ;
#23406 = SHAPE_REPRESENTATION_RELATIONSHIP ( 'NONE' , 'NONE' ,  #16640, #20459 ) ;
#23407 = CARTESIAN_POINT ( 'NONE',  ( -2.449293598294706907E-16, 4.000000000000000000, 2.175000002731188431 ) ) ;
#23408 = EDGE_CURVE ( 'NONE', #11987, #9892, #12956, .T. ) ;
#23409 = DIRECTION ( 'NONE',  ( 0.000000000000000000, 0.000000000000000000, -1.000000000000000000 ) ) ;
#23410 = ORIENTED_EDGE ( 'NONE', *, *, #7030, .T. ) ;
#23411 = EDGE_CURVE ( 'NONE', #5926, #17904, #22151, .T. ) ;
#23412 = CARTESIAN_POINT ( 'NONE',  ( -3.999999999999999112, 0.000000000000000000, 18.00000000000001066 ) ) ;
#23413 = VERTEX_POINT ( 'NONE', #9621 ) ;
#23414 = DIRECTION ( 'NONE',  ( 0.000000000000000000, 0.000000000000000000, 1.000000000000000000 ) ) ;
#23415 = DIRECTION ( 'NONE',  ( -1.000000000000000000, -0.000000000000000000, -0.000000000000000000 ) ) ;
#23416 = ORIENTED_EDGE ( 'NONE', *, *, #16360, .T. ) ;
#23417 = FACE_BOUND ( 'NONE', #13844, .T. ) ;
#23418 = CARTESIAN_POINT ( 'NONE',  ( 2.500000000000000000, -1.178949249685218748, -2.041999999999998039 ) ) ;
#23419 = PLANE ( 'NONE',  #6407 ) ;
#23420 = CARTESIAN_POINT ( 'NONE',  ( 72.00000000000000000, 8.232233047033629347, 13.23223304703362402 ) ) ;
#23421 = ADVANCED_FACE ( 'NONE', ( #20353 ), #3961, .T. ) ;
#23422 = CIRCLE ( 'NONE', #15518, 4.000000000000000000 ) ;
#23423 = CARTESIAN_POINT ( 'NONE',  ( -65.45000000218495018, 8.964466094067260471, 17.50000000000000355 ) ) ;
#23424 = AXIS2_PLACEMENT_3D ( 'NONE', #1208, #8545, #15852 ) ;
#23425 = PLANE ( 'NONE',  #17977 ) ;
#23426 = CARTESIAN_POINT ( 'NONE',  ( 57.78356816583844591, 8.275094609561968184, 11.02818770551464667 ) ) ;
#23427 = ADVANCED_FACE ( 'NONE', ( #16787 ), #368, .T. ) ;
#23428 = CARTESIAN_POINT ( 'NONE',  ( 1.432654583217642275, -3.458734124999999437, 5.050000001365596347 ) ) ;
#23429 = CARTESIAN_POINT ( 'NONE',  ( 1.432654583217643163, -3.458734124999999437, 13.75000000136560452 ) ) ;
#23430 = B_SPLINE_CURVE_WITH_KNOTS ( 'NONE', 3,
 ( #8629, #10447, #15932, #6821, #16171, #14144 ),
 .UNSPECIFIED., .F., .F.,
 ( 4, 2, 4 ),
 ( 0.006695446894088490607, 0.008593684019695168111, 0.01049192114530184475 ),
 .UNSPECIFIED. ) ;
#23431 = CARTESIAN_POINT ( 'NONE',  ( 26.04405168928502334, 7.758664279913913830, 10.00000000000008882 ) ) ;
#23432 = CARTESIAN_POINT ( 'NONE',  ( 34.67044344676619971, -9.000000000000007105, 5.000000000000079936 ) ) ;
#23433 = ORIENTED_EDGE ( 'NONE', *, *, #16015, .T. ) ;
#23434 = DIRECTION ( 'NONE',  ( 1.000000000000000000, 0.000000000000000000, 0.000000000000000000 ) ) ;
#23435 = DIRECTION ( 'NONE',  ( -1.000000000000000000, 1.776356839400250465E-15, 0.000000000000000000 ) ) ;
#23436 = CARTESIAN_POINT ( 'NONE',  ( 4.999999999999999112, -8.734705317681623171, -0.4999240074895356933 ) ) ;
#23437 = EDGE_CURVE ( 'NONE', #15099, #2752, #13209, .T. ) ;
#23438 = EDGE_CURVE ( 'NONE', #6397, #10129, #19140, .T. ) ;
#23439 = ORIENTED_EDGE ( 'NONE', *, *, #4635, .T. ) ;
#23440 = CARTESIAN_POINT ( 'NONE',  ( 4.999999999999999112, -9.241976615262146311, -1.699438267350473097 ) ) ;
#23441 = EDGE_LOOP ( 'NONE', ( #2819, #10994, #20267, #659 ) ) ;
#23442 = DIRECTION ( 'NONE',  ( 0.000000000000000000, 0.000000000000000000, 1.000000000000000000 ) ) ;
#23443 = VERTEX_POINT ( 'NONE', #22994 ) ;
#23444 = DIRECTION ( 'NONE',  ( -1.000000000000000000, 0.000000000000000000, 0.000000000000000000 ) ) ;
#23445 = VERTEX_POINT ( 'NONE', #21062 ) ;
#23446 = CARTESIAN_POINT ( 'NONE',  ( 58.53356816583845301, 11.72490539043803004, 18.97181229448534268 ) ) ;
#23447 = CARTESIAN_POINT ( 'NONE',  ( 69.45000000218493597, 8.964466094067258695, 17.50000000000000355 ) ) ;
#23448 = CARTESIAN_POINT ( 'NONE',  ( 45.00000000000000000, 10.00000000000001599, 34.11836509645781490 ) ) ;
#23449 = CARTESIAN_POINT ( 'NONE',  ( 4.999999999999999112, -2.223716399045513548, -8.461683424509336859 ) ) ;
#23450 = DIRECTION ( 'NONE',  ( 0.000000000000000000, 1.000000000000000000, -1.224646799147353207E-16 ) ) ;
#23451 = ORIENTED_EDGE ( 'NONE', *, *, #18323, .T. ) ;
#23452 = DIRECTION ( 'NONE',  ( 1.000000000000000000, 0.000000000000000000, 0.000000000000000000 ) ) ;
#23453 = CARTESIAN_POINT ( 'NONE',  ( 52.74768183416157541, 7.830560233210222876, 17.07320092032950498 ) ) ;
#23454 = CARTESIAN_POINT ( 'NONE',  ( -19.99999999999999645, -9.000000000000003553, 5.000000000000079936 ) ) ;
#23455 = CARTESIAN_POINT ( 'NONE',  ( 66.20000000109246230, 9.143825827087050939, 12.93301269999999370 ) ) ;
#23456 = DIRECTION ( 'NONE',  ( 0.000000000000000000, 0.000000000000000000, 1.000000000000000000 ) ) ;
#23457 = VECTOR ( 'NONE', #7979, 1000.000000000000000 ) ;
#23458 = DIRECTION ( 'NONE',  ( 0.000000000000000000, 0.000000000000000000, 1.000000000000000000 ) ) ;
#23459 = ORIENTED_EDGE ( 'NONE', *, *, #11731, .F. ) ;
#23460 = FACE_OUTER_BOUND ( 'NONE', #9796, .T. ) ;
#23461 = CIRCLE ( 'NONE', #2804, 4.714285714285714413 ) ;
#23462 = CARTESIAN_POINT ( 'NONE',  ( 57.37500000000000000, 7.878679656440349177, 12.87867965644035984 ) ) ;
#23463 = DIRECTION ( 'NONE',  ( 1.000000000000000000, 0.000000000000000000, 0.000000000000000000 ) ) ;
#23464 = EDGE_CURVE ( 'NONE', #17728, #17488, #17026, .T. ) ;
#23465 = EDGE_CURVE ( 'NONE', #13122, #14895, #600, .T. ) ;
#23466 = ORIENTED_EDGE ( 'NONE', *, *, #23602, .F. ) ;
#23467 = DIRECTION ( 'NONE',  ( -1.000000000000000000, -0.000000000000000000, -0.000000000000000000 ) ) ;
#23468 = CARTESIAN_POINT ( 'NONE',  ( -2.445694354108819635, -2.445694354108820523, -1.137499998634402765 ) ) ;
#23469 = PLANE ( 'NONE',  #16587 ) ;
#23470 = VERTEX_POINT ( 'NONE', #11658 ) ;
#23471 = CARTESIAN_POINT ( 'NONE',  ( -66.00000000218494733, 12.50000000000000000, 14.99999999999999645 ) ) ;
#23472 = ORIENTED_EDGE ( 'NONE', *, *, #8196, .T. ) ;
#23473 = DIRECTION ( 'NONE',  ( 1.000000000000000000, 0.000000000000000000, 0.000000000000000000 ) ) ;
#23474 = CARTESIAN_POINT ( 'NONE',  ( -2.828427124746188515, -2.828427124746190735, 17.12500000000001066 ) ) ;
#23475 = LINE ( 'NONE', #1908, #14189 ) ;
#23476 = LINE ( 'NONE', #19987, #11490 ) ;
#23477 = FACE_OUTER_BOUND ( 'NONE', #19983, .T. ) ;
#23478 = CARTESIAN_POINT ( 'NONE',  ( -66.79999999999999716, 11.76776695296636888, 16.76776695296636532 ) ) ;
#23479 = CARTESIAN_POINT ( 'NONE',  ( 2.500000000000000000, -1.178949249685214307, 2.042000000000001592 ) ) ;
#23480 = CARTESIAN_POINT ( 'NONE',  ( 60.00000000000004974, 12.90160382567056274, 16.03866470743757588 ) ) ;
#23481 = FACE_OUTER_BOUND ( 'NONE', #22063, .T. ) ;
#23482 =( BOUNDED_CURVE ( )  B_SPLINE_CURVE ( 3, ( #17092, #664, #15322, #16973 ),
 .UNSPECIFIED., .F., .F. ) 
 B_SPLINE_CURVE_WITH_KNOTS ( ( 4, 4 ),
 ( 1.570796326794896558, 1.666162211095538082 ),
 .UNSPECIFIED. ) 
 CURVE ( )  GEOMETRIC_REPRESENTATION_ITEM ( )  RATIONAL_B_SPLINE_CURVE ( ( 1.000000000000000000, 0.9992422559301721297, 0.9992422559301721297, 1.000000000000000000 ) ) 
 REPRESENTATION_ITEM ( '' )  );
#23483 = CARTESIAN_POINT ( 'NONE',  ( 1.656854249492383024, -3.999999999999999112, 5.612500000000003375 ) ) ;
#23484 = CARTESIAN_POINT ( 'NONE',  ( -2.247776618166700491, 3.308700692843503877, 10.00000000000000888 ) ) ;
#23485 = DIRECTION ( 'NONE',  ( 1.224646799147353207E-16, -0.000000000000000000, 1.000000000000000000 ) ) ;
#23486 = CARTESIAN_POINT ( 'NONE',  ( -2.445694354108818303, -2.445694354108820523, 17.56250000136560274 ) ) ;
#23487 = CARTESIAN_POINT ( 'NONE',  ( -66.20000000218495018, 9.999999999999998224, 17.49999999999999645 ) ) ;
#23488 = ORIENTED_EDGE ( 'NONE', *, *, #22567, .T. ) ;
#23489 = CARTESIAN_POINT ( 'NONE',  ( 49.55947366966726264, -11.25000000000000355, 5.000000000000079936 ) ) ;
#23490 = ORIENTED_EDGE ( 'NONE', *, *, #6855, .F. ) ;
#23491 = CARTESIAN_POINT ( 'NONE',  ( 53.96643183416157541, 6.028187705514633343, 13.27509460956200016 ) ) ;
#23492 = CARTESIAN_POINT ( 'NONE',  ( -66.95000000109246230, 11.46158073645647235, 13.53841926354352232 ) ) ;
#23493 = CARTESIAN_POINT ( 'NONE',  ( -2.445694354108820523, 2.445694354108820523, -2.387499998634403653 ) ) ;
#23494 = ORIENTED_EDGE ( 'NONE', *, *, #10533, .T. ) ;
#23495 = DIRECTION ( 'NONE',  ( -0.3420201433256622181, 0.9396926207859106484, 1.232595164407828100E-31 ) ) ;
#23496 = AXIS2_PLACEMENT_3D ( 'NONE', #20081, #18418, #1997 ) ;
#23497 = ORIENTED_EDGE ( 'NONE', *, *, #484, .T. ) ;
#23498 = CARTESIAN_POINT ( 'NONE',  ( 5.200000000000002842, 0.000000000000000000, 0.000000000000000000 ) ) ;
#23499 = VERTEX_POINT ( 'NONE', #8056 ) ;
#23500 = CARTESIAN_POINT ( 'NONE',  ( 59.34375000000000711, 8.757359312880723223, 18.00000000000000355 ) ) ;
#23501 = EDGE_CURVE ( 'NONE', #20516, #6311, #15245, .T. ) ;
#23502 = VECTOR ( 'NONE', #11330, 1000.000000000000114 ) ;
#23503 = CARTESIAN_POINT ( 'NONE',  ( -70.65000000109247935, 7.933012699999995476, 14.99999999999999645 ) ) ;
#23504 = VECTOR ( 'NONE', #8050, 1000.000000000000000 ) ;
#23505 = CARTESIAN_POINT ( 'NONE',  ( -71.20000000109246230, 12.06698730000000275, 14.14382582708705094 ) ) ;
#23506 = CARTESIAN_POINT ( 'NONE',  ( 1.872352939448454495E-15, -3.458734125000000770, 15.93750000136560629 ) ) ;
#23507 = DIRECTION ( 'NONE',  ( 0.000000000000000000, -0.9510565162951500895, -0.3090169943749582204 ) ) ;
#23508 = CARTESIAN_POINT ( 'NONE',  ( 54.37500000000000711, 7.878679656440349177, 12.87867965644035984 ) ) ;
#23509 = FACE_OUTER_BOUND ( 'NONE', #12015, .T. ) ;
#23510 = CARTESIAN_POINT ( 'NONE',  ( 59.43750000000000711, 10.00000000000000711, 17.99999999999999645 ) ) ;
#23511 = DIRECTION ( 'NONE',  ( -1.000000000000000000, -7.703719777548943412E-32, 0.000000000000000000 ) ) ;
#23512 = CARTESIAN_POINT ( 'NONE',  ( 2.828427124746192067, -2.828427124746189847, 18.50000000273119483 ) ) ;
#23513 = FACE_BOUND ( 'NONE', #7561, .T. ) ;
#23514 = VECTOR ( 'NONE', #14832, 1000.000000000000000 ) ;
#23515 = VERTEX_POINT ( 'NONE', #8409 ) ;
#23516 = DIRECTION ( 'NONE',  ( 0.000000000000000000, 0.000000000000000000, 1.000000000000000000 ) ) ;
#23517 = CYLINDRICAL_SURFACE ( 'NONE', #8615, 11.00000000000000000 ) ;
#23518 = VERTEX_POINT ( 'NONE', #6241 ) ;
#23519 = CARTESIAN_POINT ( 'NONE',  ( 53.15625000000001421, 7.000000000000003553, 16.24264068711929099 ) ) ;
#23520 = VECTOR ( 'NONE', #21417, 1000.000000000000000 ) ;
#23521 = SURFACE_SIDE_STYLE ('',( #8942 ) ) ;
#23522 = CARTESIAN_POINT ( 'NONE',  ( 7.347880794884118750E-16, -4.000000000000000000, 0.6750000027311870987 ) ) ;
#23523 = AXIS2_PLACEMENT_3D ( 'NONE', #18530, #8137, #805 ) ;
#23524 = LINE ( 'NONE', #21841, #19696 ) ;
#23525 = ORIENTED_EDGE ( 'NONE', *, *, #11990, .F. ) ;
#23526 = CARTESIAN_POINT ( 'NONE',  ( -1.656854249492379250, 4.000000000000000000, 17.81250000000001421 ) ) ;
#23527 = VERTEX_POINT ( 'NONE', #12122 ) ;
#23528 =( BOUNDED_SURFACE ( )  B_SPLINE_SURFACE ( 3, 2, ( 
 ( #459, #14740, #334 ),
 ( #22000, #5613, #11150 ),
 ( #9700, #9345, #16633 ),
 ( #18660, #211, #7542 ),
 ( #2247, #2368, #3925 ),
 ( #20563, #7668, #14861 ) ),
 .UNSPECIFIED., .F., .F., .F. ) 
 B_SPLINE_SURFACE_WITH_KNOTS ( ( 4, 2, 4 ),
 ( 3, 3 ),
 ( 0.02027752710269158445, 0.02273781595091097299, 0.02519810479913036153 ),
 ( 0.000000000000000000, 1.000000000000000000 ),
 .UNSPECIFIED. ) 
 GEOMETRIC_REPRESENTATION_ITEM ( )  RATIONAL_B_SPLINE_SURFACE ( (
 ( 1.000000000000000000, 0.8047781431712808242, 1.000000000000000000),
 ( 1.000000000000000000, 0.8123773247083928561, 1.000000000000000000),
 ( 1.000000000000000000, 0.8190670192154906326, 1.000000000000000000),
 ( 1.000000000000000000, 0.8192353552912178261, 1.000000000000000000),
 ( 1.000000000000000000, 0.8126132098226825917, 1.000000000000000000),
 ( 1.000000000000000000, 0.8047712465856394770, 1.000000000000000000) ) ) 
 REPRESENTATION_ITEM ( '' )  SURFACE ( )  );
#23529 = CARTESIAN_POINT ( 'NONE',  ( 3.869372803233808611, -9.000000000000001776, 10.00000000000008882 ) ) ;
#23530 = PLANE ( 'NONE',  #19053 ) ;
#23531 = ORIENTED_EDGE ( 'NONE', *, *, #2796, .T. ) ;
#23532 = DIRECTION ( 'NONE',  ( -0.000000000000000000, -1.000000000000000000, -0.000000000000000000 ) ) ;
#23533 = EDGE_CURVE ( 'NONE', #17270, #22762, #5380, .T. ) ;
#23534 = CARTESIAN_POINT ( 'NONE',  ( 0.000000000000000000, 4.057423117305393845, 8.475820894092990443 ) ) ;
#23535 = EDGE_CURVE ( 'NONE', #6666, #19611, #9730, .T. ) ;
#23536 = ORIENTED_EDGE ( 'NONE', *, *, #723, .T. ) ;
#23537 = CARTESIAN_POINT ( 'NONE',  ( -3.999999999999999112, 0.000000000000000000, 14.00000000000001066 ) ) ;
#23538 = CIRCLE ( 'NONE', #11333, 4.000000000000001776 ) ;
#23539 = CARTESIAN_POINT ( 'NONE',  ( 71.39999999999999147, 11.76776695296636888, 13.23223304703362579 ) ) ;
#23540 = AXIS2_PLACEMENT_3D ( 'NONE', #11377, #18657, #2244 ) ;
#23541 = EDGE_CURVE ( 'NONE', #1835, #4715, #4439, .T. ) ;
#23542 = CARTESIAN_POINT ( 'NONE',  ( -3.999999999999998224, -1.656854249492383024, 17.18750000273119838 ) ) ;
#23543 = CARTESIAN_POINT ( 'NONE',  ( 4.999999999999999112, 8.461683424509315543, 2.223716399045600145 ) ) ;
#23544 = CARTESIAN_POINT ( 'NONE',  ( 57.22106816583844591, 14.02818770551465377, 16.58880310854672757 ) ) ;
#23545 = CARTESIAN_POINT ( 'NONE',  ( -3.458734125000000326, 1.432654583217640276, 1.675000001365597235 ) ) ;
#23546 = FACE_OUTER_BOUND ( 'NONE', #15995, .T. ) ;
#23547 = CARTESIAN_POINT ( 'NONE',  ( 1.432654583217643163, -3.458734124999999437, 16.75000000136560629 ) ) ;
#23548 = CARTESIAN_POINT ( 'NONE',  ( -12.45344630323380031, -9.000000000000003553, 5.000000000000079936 ) ) ;
#23549 = VECTOR ( 'NONE', #13535, 1000.000000000000000 ) ;
#23550 = VECTOR ( 'NONE', #7042, 1000.000000000000000 ) ;
#23551 = CARTESIAN_POINT ( 'NONE',  ( 7.010965453233809264, -9.000000000000001776, 5.000000000000079936 ) ) ;
#23552 = VERTEX_POINT ( 'NONE', #11773 ) ;
#23553 = LINE ( 'NONE', #10536, #1142 ) ;
#23554 = CARTESIAN_POINT ( 'NONE',  ( 68.24999999999998579, 12.50000000000000000, 13.96446609406725692 ) ) ;
#23555 = CARTESIAN_POINT ( 'NONE',  ( -6.499999999999999112, 7.960204194457794491E-16, 9.480888224575631185 ) ) ;
#23556 = VERTEX_POINT ( 'NONE', #15370 ) ;
#23557 = ORIENTED_EDGE ( 'NONE', *, *, #8449, .T. ) ;
#23558 = FACE_BOUND ( 'NONE', #3557, .T. ) ;
#23559 = AXIS2_PLACEMENT_3D ( 'NONE', #15255, #6011, #843 ) ;
#23560 = EDGE_CURVE ( 'NONE', #7525, #11761, #2987, .T. ) ;
#23561 = ORIENTED_EDGE ( 'NONE', *, *, #22978, .F. ) ;
#23562 = CARTESIAN_POINT ( 'NONE',  ( 57.56250000000000000, 5.999999999999996447, 15.00000000000001599 ) ) ;
#23563 = ORIENTED_EDGE ( 'NONE', *, *, #18619, .T. ) ;
#23564 = CARTESIAN_POINT ( 'NONE',  ( -3.999999999999999112, 0.000000000000000000, 18.00000000000001066 ) ) ;
#23565 = ORIENTED_EDGE ( 'NONE', *, *, #1907, .F. ) ;
#23566 = CARTESIAN_POINT ( 'NONE',  ( 54.00000000000000711, 12.82842712474617741, 12.17157287525379239 ) ) ;
#23567 = EDGE_CURVE ( 'NONE', #589, #17422, #20715, .T. ) ;
#23568 = CARTESIAN_POINT ( 'NONE',  ( 69.40000000218495302, 9.999999999999998224, 17.49999999999999645 ) ) ;
#23569 = DIRECTION ( 'NONE',  ( -1.000000000000000000, -7.703719777548943412E-32, 0.000000000000000000 ) ) ;
#23570 = DIRECTION ( 'NONE',  ( 6.123233995736827666E-17, -1.000000000000000000, 0.000000000000000000 ) ) ;
#23571 = DIRECTION ( 'NONE',  ( -1.000000000000000000, -0.000000000000000000, -0.000000000000000000 ) ) ;
#23572 = ADVANCED_FACE ( 'NONE', ( #2751 ), #2513, .F. ) ;
#23573 = ORIENTED_EDGE ( 'NONE', *, *, #7239, .F. ) ;
#23574 = CARTESIAN_POINT ( 'NONE',  ( -3.999999999999999112, 0.000000000000000000, 18.12500000273119483 ) ) ;
#23575 = EDGE_CURVE ( 'NONE', #9212, #9912, #5331, .T. ) ;
#23576 = CARTESIAN_POINT ( 'NONE',  ( 2.499999999999999556, -1.975651141462315463, 10.82112760146735475 ) ) ;
#23577 = CARTESIAN_POINT ( 'NONE',  ( 51.99768183416157541, 12.16943976678977535, 12.92679907967048614 ) ) ;
#23578 = FACE_OUTER_BOUND ( 'NONE', #10394, .T. ) ;
#23579 = CARTESIAN_POINT ( 'NONE',  ( 67.60000000109246798, 7.933012699999995476, 15.85617417291294196 ) ) ;
#23580 = CARTESIAN_POINT ( 'NONE',  ( -0.5316568767328819778, -7.198601258566901251, -0.4033376246892538264 ) ) ;
#23581 = LINE ( 'NONE', #7191, #8870 ) ;
#23582 = ORIENTED_EDGE ( 'NONE', *, *, #7023, .T. ) ;
#23583 = CARTESIAN_POINT ( 'NONE',  ( 1.236993788156008760E-15, 0.000000000000000000, 21.31370849898476649 ) ) ;
#23584 = CARTESIAN_POINT ( 'NONE',  ( 58.78125000000000711, 8.757359312880703683, 11.99999999999999822 ) ) ;
#23585 = CARTESIAN_POINT ( 'NONE',  ( -20.00000000000001066, 7.500000000000001776, -49.99999999999999289 ) ) ;
#23586 = ORIENTED_EDGE ( 'NONE', *, *, #7212, .F. ) ;
#23587 = CARTESIAN_POINT ( 'NONE',  ( 28.38725814676620018, -9.000000000000003553, 5.000000000000079936 ) ) ;
#23588 = CARTESIAN_POINT ( 'NONE',  ( -2.445694354108819635, -2.445694354108820523, -2.137499998634403653 ) ) ;
#23589 = LINE ( 'NONE', #6717, #8242 ) ;
#23590 = ORIENTED_EDGE ( 'NONE', *, *, #13154, .T. ) ;
#23591 = DIRECTION ( 'NONE',  ( -1.000000000000000000, 0.000000000000000000, 0.000000000000000000 ) ) ;
#23592 = ORIENTED_EDGE ( 'NONE', *, *, #3095, .F. ) ;
#23593 = CARTESIAN_POINT ( 'NONE',  ( 2.499999999999999556, 9.915734732513284300, -4.762163868918174892 ) ) ;
#23594 = AXIS2_PLACEMENT_3D ( 'NONE', #269, #3872, #7376 ) ;
#23595 = CARTESIAN_POINT ( 'NONE',  ( -3.999999999999999112, 1.656854249492380804, 16.93750000000001066 ) ) ;
#23596 = DIRECTION ( 'NONE',  ( 0.000000000000000000, -1.000000000000000000, 0.000000000000000000 ) ) ;
#23597 = CARTESIAN_POINT ( 'NONE',  ( 1.520000000000000462, 0.000000000000000000, 0.000000000000000000 ) ) ;
#23598 = EDGE_CURVE ( 'NONE', #17065, #13999, #8464, .T. ) ;
#23599 = EDGE_CURVE ( 'NONE', #3988, #6515, #23344, .T. ) ;
#23600 = CARTESIAN_POINT ( 'NONE',  ( -2.449848172108560540, -3.432307619358754724, -3.503702292528910078 ) ) ;
#23601 = AXIS2_PLACEMENT_3D ( 'NONE', #8538, #20954, #21078 ) ;
#23602 = EDGE_CURVE ( 'NONE', #12158, #17853, #17380, .T. ) ;
#23603 = CARTESIAN_POINT ( 'NONE',  ( -67.89999999999999147, 7.499999999999996447, 14.99999999999999645 ) ) ;
#23604 = CARTESIAN_POINT ( 'NONE',  ( 45.00000000000000000, -14.69846310392956745, 35.82846581308617573 ) ) ;
#23605 = CARTESIAN_POINT ( 'NONE',  ( -3.458734124999998993, 1.432654583217640276, 17.37500000136559919 ) ) ;
#23606 = DIRECTION ( 'NONE',  ( 0.000000000000000000, 0.000000000000000000, -1.000000000000000000 ) ) ;
#23607 = CARTESIAN_POINT ( 'NONE',  ( -4.000000000000000888, 1.656854249492380804, 5.237500000000000711 ) ) ;
#23608 = CARTESIAN_POINT ( 'NONE',  ( -66.60000000109246798, 10.85617417291294551, 17.06698730000000097 ) ) ;
#23609 = CARTESIAN_POINT ( 'NONE',  ( 68.25000000218493312, 11.03553390593269157, 12.49999999999994849 ) ) ;
#23610 = CARTESIAN_POINT ( 'NONE',  ( -1.432654583217638944, 3.458734125000000326, 19.25000000136560274 ) ) ;
#23611 = CARTESIAN_POINT ( 'NONE',  ( -66.45000000218495018, 7.499999999999996447, 13.96446609406725514 ) ) ;
#23612 = ORIENTED_EDGE ( 'NONE', *, *, #6031, .F. ) ;
#23613 =( GEOMETRIC_REPRESENTATION_CONTEXT ( 3 ) GLOBAL_UNCERTAINTY_ASSIGNED_CONTEXT ( ( #2352 ) ) GLOBAL_UNIT_ASSIGNED_CONTEXT ( ( #20701, #474, #15355 ) ) REPRESENTATION_CONTEXT ( 'NONE', 'WORKASPACE' ) );
#23614 = CARTESIAN_POINT ( 'NONE',  ( -70.50000000109247367, 9.143825827087049163, 17.06698730000000097 ) ) ;
#23615 = EDGE_LOOP ( 'NONE', ( #2378, #8644 ) ) ;
#23616 = CARTESIAN_POINT ( 'NONE',  ( 52.74768183416157541, 7.123453452023678523, 17.78030770151605822 ) ) ;
#23617 = CARTESIAN_POINT ( 'NONE',  ( -65.90000000109246514, 7.933012699999995476, 14.14382582708705094 ) ) ;
#23618 = CARTESIAN_POINT ( 'NONE',  ( 0.000000000000000000, 0.000000000000000000, 0.000000000000000000 ) ) ;
#23619 = ADVANCED_BREP_SHAPE_REPRESENTATION ( '', ( #22323, #7318 ), #9953 ) ;
#23620 = CARTESIAN_POINT ( 'NONE',  ( 2.445694354108820079, 2.445694354108820523, -2.637499998634404097 ) ) ;
#23621 = ORIENTED_EDGE ( 'NONE', *, *, #7164, .T. ) ;
#23622 = VECTOR ( 'NONE', #17455, 1000.000000000000114 ) ;
#23623 = ORIENTED_EDGE ( 'NONE', *, *, #15954, .F. ) ;
#23624 = CARTESIAN_POINT ( 'NONE',  ( -3.458734124999999437, 1.432654583217640498, 19.62500000136560629 ) ) ;
#23625 = CARTESIAN_POINT ( 'NONE',  ( 59.53125000000000000, 11.24264068711929276, 18.00000000000000355 ) ) ;
#23626 = CARTESIAN_POINT ( 'NONE',  ( -72.00000000109248788, 10.85617417291294551, 17.06698729999999742 ) ) ;
#23627 = EDGE_CURVE ( 'NONE', #13955, #8977, #19273, .T. ) ;
#23628 = AXIS2_PLACEMENT_3D ( 'NONE', #21159, #17719, #6813 ) ;
#23629 = CARTESIAN_POINT ( 'NONE',  ( -69.25000000109245946, 7.933012699999995476, 14.99999999999999645 ) ) ;
#23630 =( BOUNDED_CURVE ( )  B_SPLINE_CURVE ( 2, ( #11943, #2685, #2795, #10025, #13495, #15295, #17312, #20647, #19208 ),
 .UNSPECIFIED., .F., .F. ) 
 B_SPLINE_CURVE_WITH_KNOTS ( ( 3, 2, 2, 2, 3 ),
 ( 0.4500000000000000111, 0.4625000000000000222, 0.4749999999999999778, 0.4874999999999999889, 0.5000000000000000000 ),
 .UNSPECIFIED. ) 
 CURVE ( )  GEOMETRIC_REPRESENTATION_ITEM ( )  RATIONAL_B_SPLINE_CURVE ( ( 1.000000000000000000, 0.9238795325112867385, 1.000000000000000000, 0.9238795325112867385, 1.000000000000000000, 0.9238795325112867385, 1.000000000000000000, 0.9238795325112867385, 1.000000000000000000 ) ) 
 REPRESENTATION_ITEM ( '' )  );
#23631 = CARTESIAN_POINT ( 'NONE',  ( -3.458734124999999437, 0.000000000000000000, 16.68750000136560629 ) ) ;
#23632 = CARTESIAN_POINT ( 'NONE',  ( 4.000000000000000888, 1.656854249492381248, 11.68750000273119660 ) ) ;
#23633 = CARTESIAN_POINT ( 'NONE',  ( 51.28125000000000000, 8.757359312880703683, 11.99999999999999822 ) ) ;
#23634 = LINE ( 'NONE', #1591, #5263 ) ;
#23635 = CIRCLE ( 'NONE', #5275, 2.500000000000002220 ) ;
#23636 = AXIS2_PLACEMENT_3D ( 'NONE', #5805, #12892, #7385 ) ;
#23637 = CARTESIAN_POINT ( 'NONE',  ( 52.03124999999999289, 11.24264068711929276, 18.00000000000000355 ) ) ;
#23638 = LINE ( 'NONE', #6887, #1254 ) ;
#23639 = CARTESIAN_POINT ( 'NONE',  ( -68.24999999999998579, 12.50000000000000000, 13.96446609406725692 ) ) ;
#23640 = ORIENTED_EDGE ( 'NONE', *, *, #22684, .T. ) ;
#23641 = FACE_OUTER_BOUND ( 'NONE', #11582, .T. ) ;
#23642 = LINE ( 'NONE', #15997, #21570 ) ;
#23643 = ORIENTED_EDGE ( 'NONE', *, *, #18915, .T. ) ;
#23644 = CARTESIAN_POINT ( 'NONE',  ( 55.96875000000000000, 6.999999999999992895, 13.75735931288071967 ) ) ;
#23645 = CARTESIAN_POINT ( 'NONE',  ( 1.432654583217642275, -3.458734124999999437, 5.050000001365596347 ) ) ;
#23646 = CYLINDRICAL_SURFACE ( 'NONE', #9388, 4.000000000000000000 ) ;
#23647 = ORIENTED_EDGE ( 'NONE', *, *, #18986, .T. ) ;
#23648 = CARTESIAN_POINT ( 'NONE',  ( 4.000000000000001776, -1.656854249492379694, 18.43750000000000711 ) ) ;
#23649 = ORIENTED_EDGE ( 'NONE', *, *, #270, .T. ) ;
#23650 = AXIS2_PLACEMENT_3D ( 'NONE', #15585, #10075, #11988 ) ;
#23651 = CARTESIAN_POINT ( 'NONE',  ( -19.99999999999999645, -15.00000000000001954, 5.000000000000079936 ) ) ;
#23652 = DIRECTION ( 'NONE',  ( 0.000000000000000000, 0.000000000000000000, 1.000000000000000000 ) ) ;
#23653 = ORIENTED_EDGE ( 'NONE', *, *, #6862, .T. ) ;
#23654 = FACE_OUTER_BOUND ( 'NONE', #19681, .T. ) ;
#23655 = VECTOR ( 'NONE', #17767, 1000.000000000000000 ) ;
#23656 = VECTOR ( 'NONE', #21261, 1000.000000000000114 ) ;
#23657 = CARTESIAN_POINT ( 'NONE',  ( 51.00000000000000711, 12.12132034355963484, 12.87867965644034740 ) ) ;
#23658 = CARTESIAN_POINT ( 'NONE',  ( -1.432654583217640498, 3.458734125000000770, 1.800000001365597235 ) ) ;
#23659 = CARTESIAN_POINT ( 'NONE',  ( 70.25000000000000000, 7.499999999999995559, 16.03553390593273420 ) ) ;
#23660 = DIRECTION ( 'NONE',  ( -0.000000000000000000, -0.000000000000000000, -1.000000000000000000 ) ) ;
#23661 = AXIS2_PLACEMENT_3D ( 'NONE', #5369, #23571, #5482 ) ;
#23662 = CARTESIAN_POINT ( 'NONE',  ( 69.64999999999997726, 8.964466094067285340, 12.49999999999996980 ) ) ;
#23663 = CARTESIAN_POINT ( 'NONE',  ( 52.81481816583844591, 14.00000000000000178, 14.93194885905434610 ) ) ;
#23664 = CARTESIAN_POINT ( 'NONE',  ( -3.458734124999999882, -1.432654583217642497, -0.1999999986344043745 ) ) ;
#23665 = CARTESIAN_POINT ( 'NONE',  ( 0.000000000000000000, -0.4999240074895051067, 8.734705317681624948 ) ) ;
#23666 =( BOUNDED_CURVE ( )  B_SPLINE_CURVE ( 2, ( #17842, #17732, #23348, #1296, #21651, #2979, #19743, #21285, #1411 ),
 .UNSPECIFIED., .F., .F. ) 
 B_SPLINE_CURVE_WITH_KNOTS ( ( 3, 2, 2, 2, 3 ),
 ( 0.8749999999999990008, 0.8906249999999994449, 0.9062499999999998890, 0.9218750000000003331, 0.9375000000000007772 ),
 .UNSPECIFIED. ) 
 CURVE ( )  GEOMETRIC_REPRESENTATION_ITEM ( )  RATIONAL_B_SPLINE_CURVE ( ( 1.000000000000004885, 0.9238795325112818535, 1.000000000000000000, 0.9238795325112867385, 1.000000000000000000, 0.9238795325112867385, 1.000000000000000000, 0.9238795325112829637, 1.000000000000003775 ) ) 
 REPRESENTATION_ITEM ( '' )  );
#23667 = EDGE_CURVE ( 'NONE', #12703, #15725, #12482, .T. ) ;
#23668 = DIRECTION ( 'NONE',  ( 0.000000000000000000, 0.8090169943749446757, 0.5877852522924770229 ) ) ;
#23669 = ORIENTED_EDGE ( 'NONE', *, *, #16484, .F. ) ;
#23670 = CARTESIAN_POINT ( 'NONE',  ( 2.828427124746191179, 2.828427124746190291, 11.75000000273119660 ) ) ;
#23671 = AXIS2_PLACEMENT_3D ( 'NONE', #5594, #1638, #3789 ) ;
#23672 = DIRECTION ( 'NONE',  ( -1.000000000000000000, -0.000000000000000000, -0.000000000000000000 ) ) ;
#23673 = DIRECTION ( 'NONE',  ( 0.000000000000000000, 1.000000000000000000, 0.000000000000000000 ) ) ;
#23674 = ORIENTED_EDGE ( 'NONE', *, *, #22533, .T. ) ;
#23675 = ORIENTED_EDGE ( 'NONE', *, *, #9830, .T. ) ;
#23676 = CARTESIAN_POINT ( 'NONE',  ( 4.000000000000000888, 1.656854249492381248, 13.68750000273119483 ) ) ;
#23677 = ORIENTED_EDGE ( 'NONE', *, *, #20068, .T. ) ;
#23678 = AXIS2_PLACEMENT_3D ( 'NONE', #19761, #10353, #8541 ) ;
#23679 = EDGE_CURVE ( 'NONE', #19575, #9029, #17626, .T. ) ;
#23680 = CARTESIAN_POINT ( 'NONE',  ( 55.31250000000000711, 14.00000000000000000, 14.99999999999997691 ) ) ;
#23681 = ORIENTED_EDGE ( 'NONE', *, *, #15861, .F. ) ;
#23682 = DIRECTION ( 'NONE',  ( -0.000000000000000000, -0.000000000000000000, 1.000000000000000000 ) ) ;
#23683 = VERTEX_POINT ( 'NONE', #8525 ) ;
#23684 = VECTOR ( 'NONE', #3914, 1000.000000000000000 ) ;
#23685 = CARTESIAN_POINT ( 'NONE',  ( 53.56481816583844591, 5.999999999999996447, 15.06805114094564502 ) ) ;
#23686 = CARTESIAN_POINT ( 'NONE',  ( 68.55000000218495870, 11.03553390593273598, 17.50000000000000355 ) ) ;
#23687 = AXIS2_PLACEMENT_3D ( 'NONE', #13561, #22637, #9847 ) ;
#23688 = CARTESIAN_POINT ( 'NONE',  ( 0.000000000000000000, -1.178949249685214307, 2.042000000000001592 ) ) ;
#23689 = CARTESIAN_POINT ( 'NONE',  ( -68.84999999999998010, 8.964466094067214286, 12.50000000000004086 ) ) ;
#23690 = DIRECTION ( 'NONE',  ( -0.000000000000000000, -0.000000000000000000, 1.000000000000000000 ) ) ;
#23691 = EDGE_LOOP ( 'NONE', ( #17424, #16886, #14615, #979 ) ) ;
#23692 = CARTESIAN_POINT ( 'NONE',  ( 9.920644283265380691E-16, 4.000000000000000000, 16.87500000273119838 ) ) ;
#23693 = CARTESIAN_POINT ( 'NONE',  ( 18.96248019676619734, -9.000000000000003553, 5.000000000000079936 ) ) ;
#23694 = CARTESIAN_POINT ( 'NONE',  ( 59.68518183416157541, 10.06805114094561659, 10.99999999999999645 ) ) ;
#23695 = LINE ( 'NONE', #16746, #6173 ) ;
#23696 = CIRCLE ( 'NONE', #13772, 2.500000000000000444 ) ;
#23697 = DIRECTION ( 'NONE',  ( 1.000000000000000000, 0.000000000000000000, 0.000000000000000000 ) ) ;
#23698 = NEXT_ASSEMBLY_USAGE_OCCURRENCE ( 'NAUO1', ' ', ' ', #10500, #18958, $ ) ;
#23699 = NEXT_ASSEMBLY_USAGE_OCCURRENCE ( 'NAUO2', ' ', ' ', #10500, #3726, $ ) ;
#23700 = NEXT_ASSEMBLY_USAGE_OCCURRENCE ( 'NAUO3', ' ', ' ', #10500, #3726, $ ) ;
#23701 = NEXT_ASSEMBLY_USAGE_OCCURRENCE ( 'NAUO4', ' ', ' ', #10500, #2996, $ ) ;
#23702 = NEXT_ASSEMBLY_USAGE_OCCURRENCE ( 'NAUO5', ' ', ' ', #10500, #6539, $ ) ;
#23703 = NEXT_ASSEMBLY_USAGE_OCCURRENCE ( 'NAUO6', ' ', ' ', #10500, #20705, $ ) ;
#23704 = NEXT_ASSEMBLY_USAGE_OCCURRENCE ( 'NAUO7', ' ', ' ', #10500, #2996, $ ) ;
#23705 = NEXT_ASSEMBLY_USAGE_OCCURRENCE ( 'NAUO8', ' ', ' ', #10500, #7275, $ ) ;
#23706 = NEXT_ASSEMBLY_USAGE_OCCURRENCE ( 'NAUO9', ' ', ' ', #10500, #6539, $ ) ;
#23707 = NEXT_ASSEMBLY_USAGE_OCCURRENCE ( 'NAUO10', ' ', ' ', #10500, #6539, $ ) ;
#23708 = NEXT_ASSEMBLY_USAGE_OCCURRENCE ( 'NAUO11', ' ', ' ', #10500, #6539, $ ) ;
#23709 = NEXT_ASSEMBLY_USAGE_OCCURRENCE ( 'NAUO12', ' ', ' ', #10500, #520, $ ) ;
#23710 = NEXT_ASSEMBLY_USAGE_OCCURRENCE ( 'NAUO13', ' ', ' ', #10500, #13574, $ ) ;
#23711 = NEXT_ASSEMBLY_USAGE_OCCURRENCE ( 'NAUO14', ' ', ' ', #10500, #10803, $ ) ;
#23712 = NEXT_ASSEMBLY_USAGE_OCCURRENCE ( 'NAUO15', ' ', ' ', #10500, #10803, $ ) ;
#23713 = NEXT_ASSEMBLY_USAGE_OCCURRENCE ( 'NAUO16', ' ', ' ', #10500, #9760, $ ) ;
#23714 = NEXT_ASSEMBLY_USAGE_OCCURRENCE ( 'NAUO17', ' ', ' ', #10500, #9760, $ ) ;
#23715 = NEXT_ASSEMBLY_USAGE_OCCURRENCE ( 'NAUO18', ' ', ' ', #10500, #9760, $ ) ;
#23716 = NEXT_ASSEMBLY_USAGE_OCCURRENCE ( 'NAUO19', ' ', ' ', #10500, #9760, $ ) ;
#23717 = NEXT_ASSEMBLY_USAGE_OCCURRENCE ( 'NAUO20', ' ', ' ', #10500, #9760, $ ) ;
#23718 = NEXT_ASSEMBLY_USAGE_OCCURRENCE ( 'NAUO21', ' ', ' ', #10500, #9760, $ ) ;
ENDSEC;
END-ISO-10303-21;
